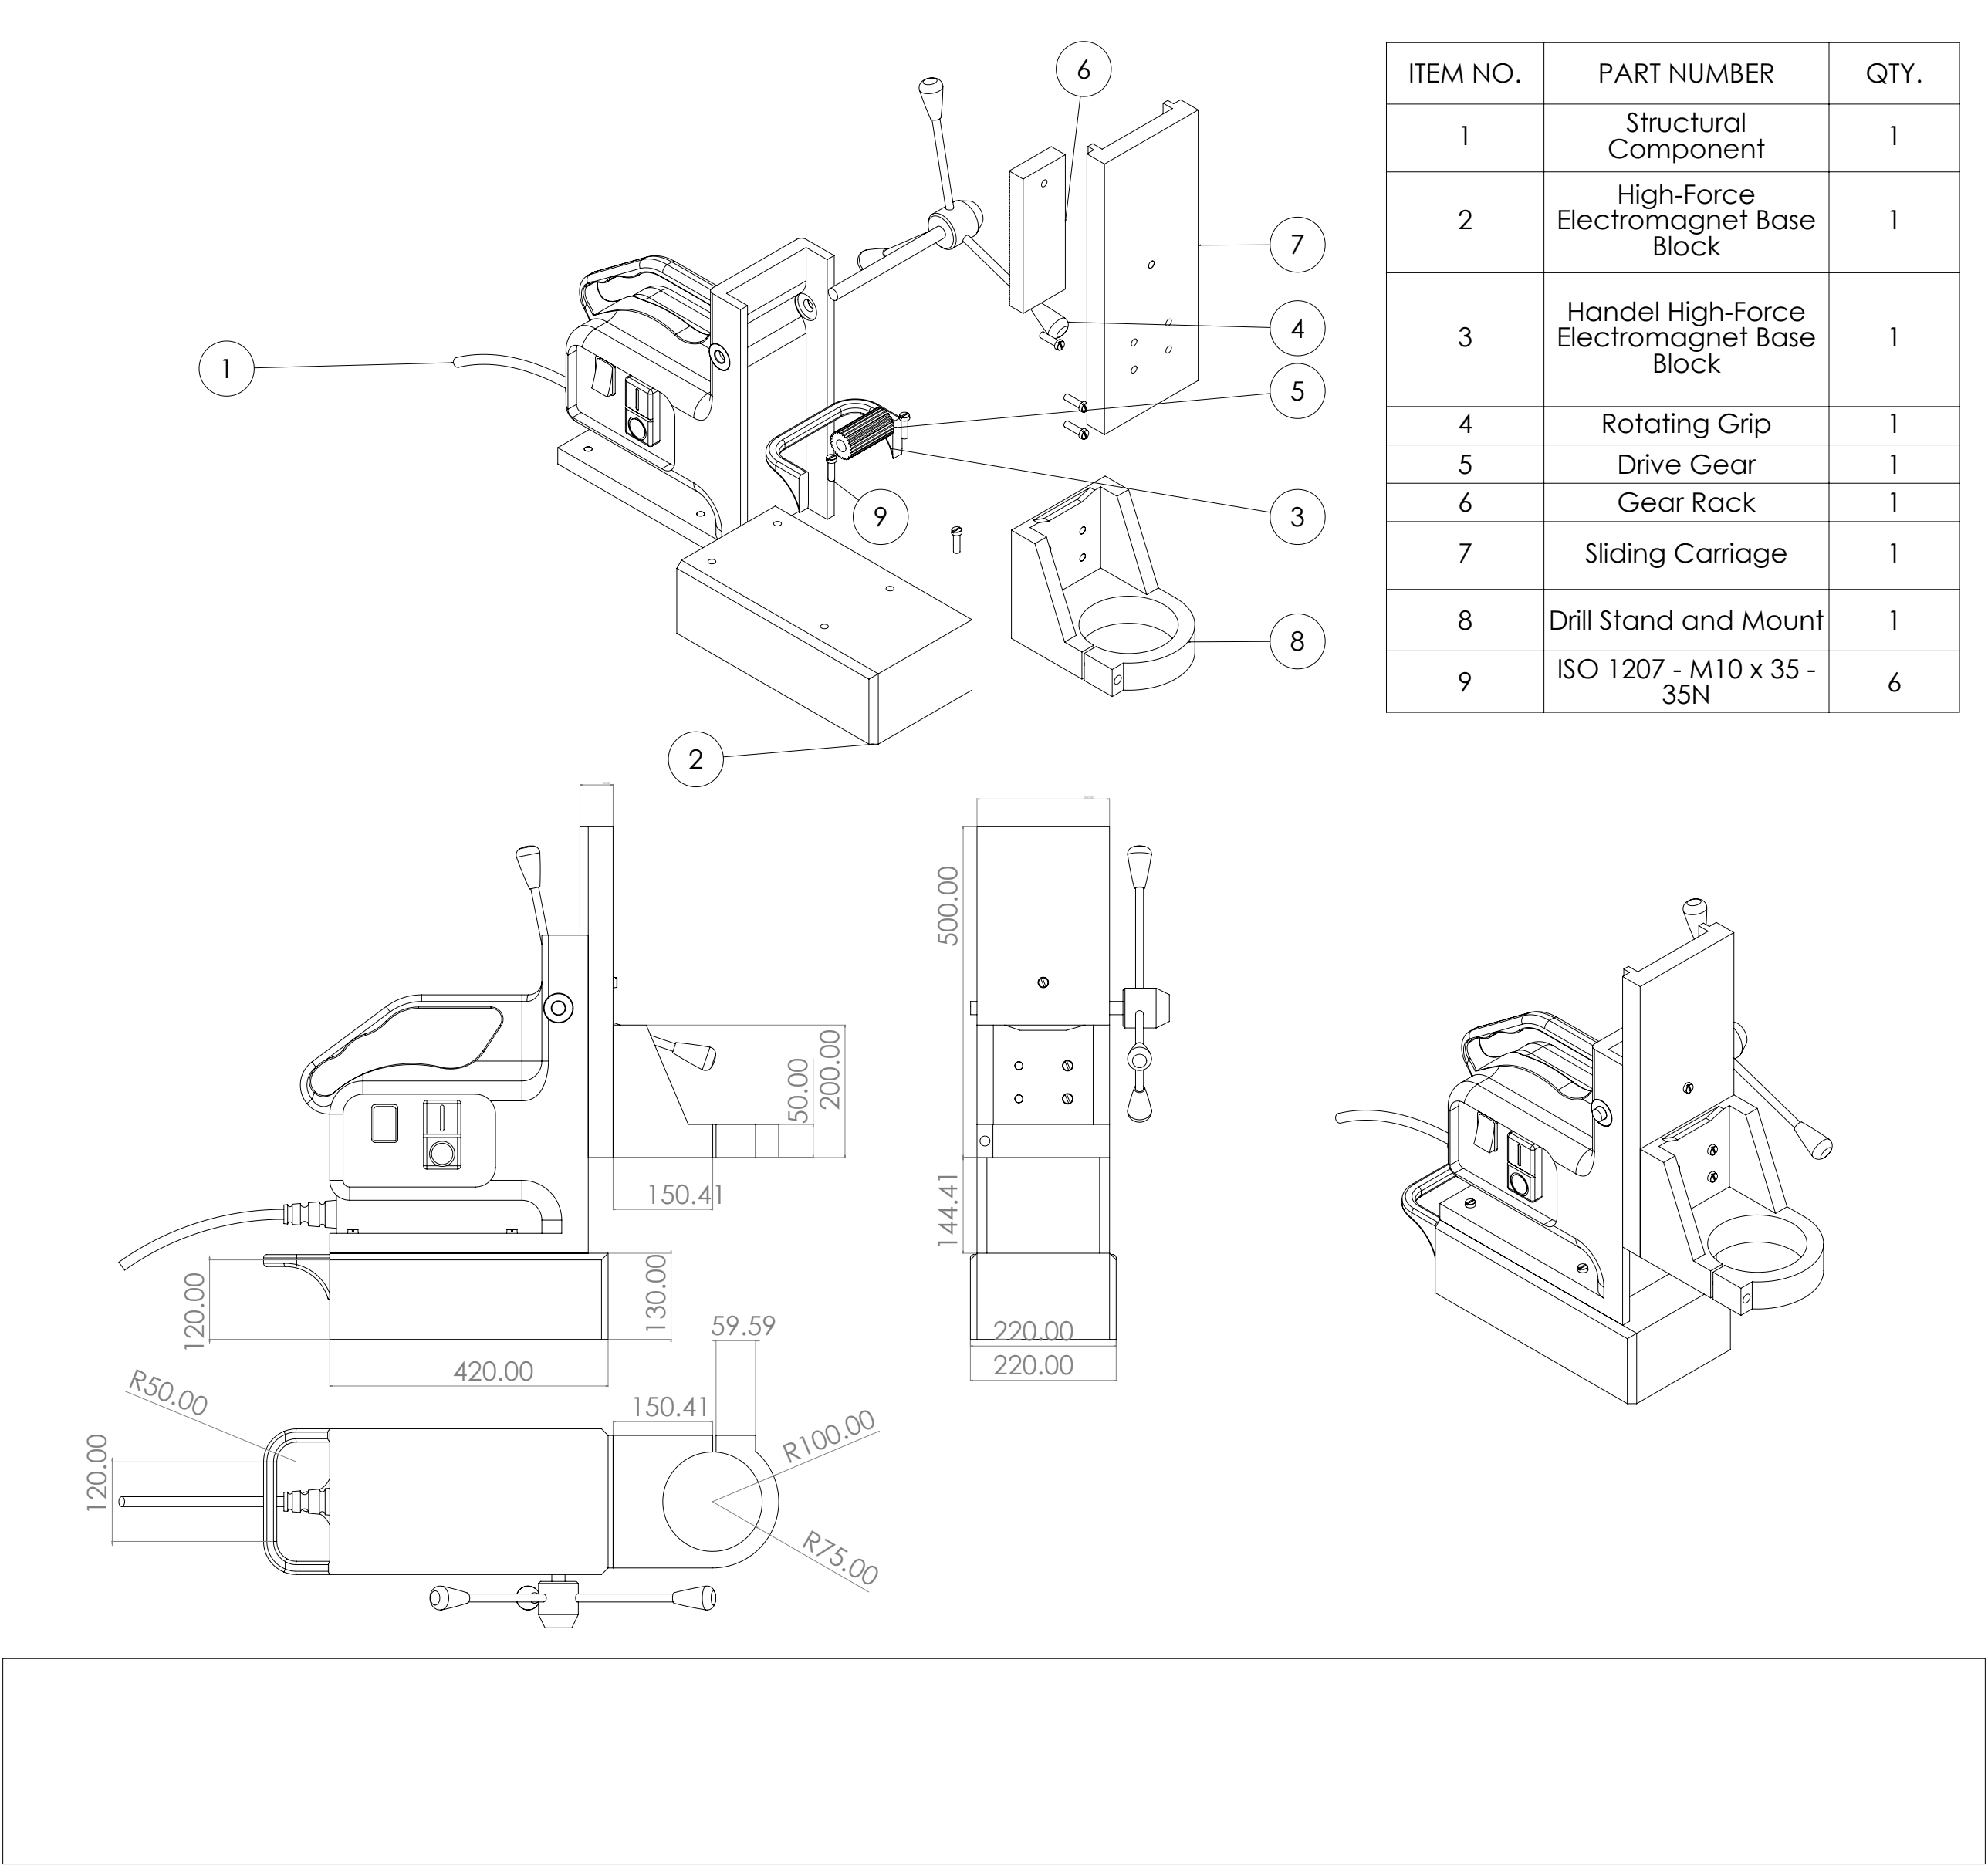
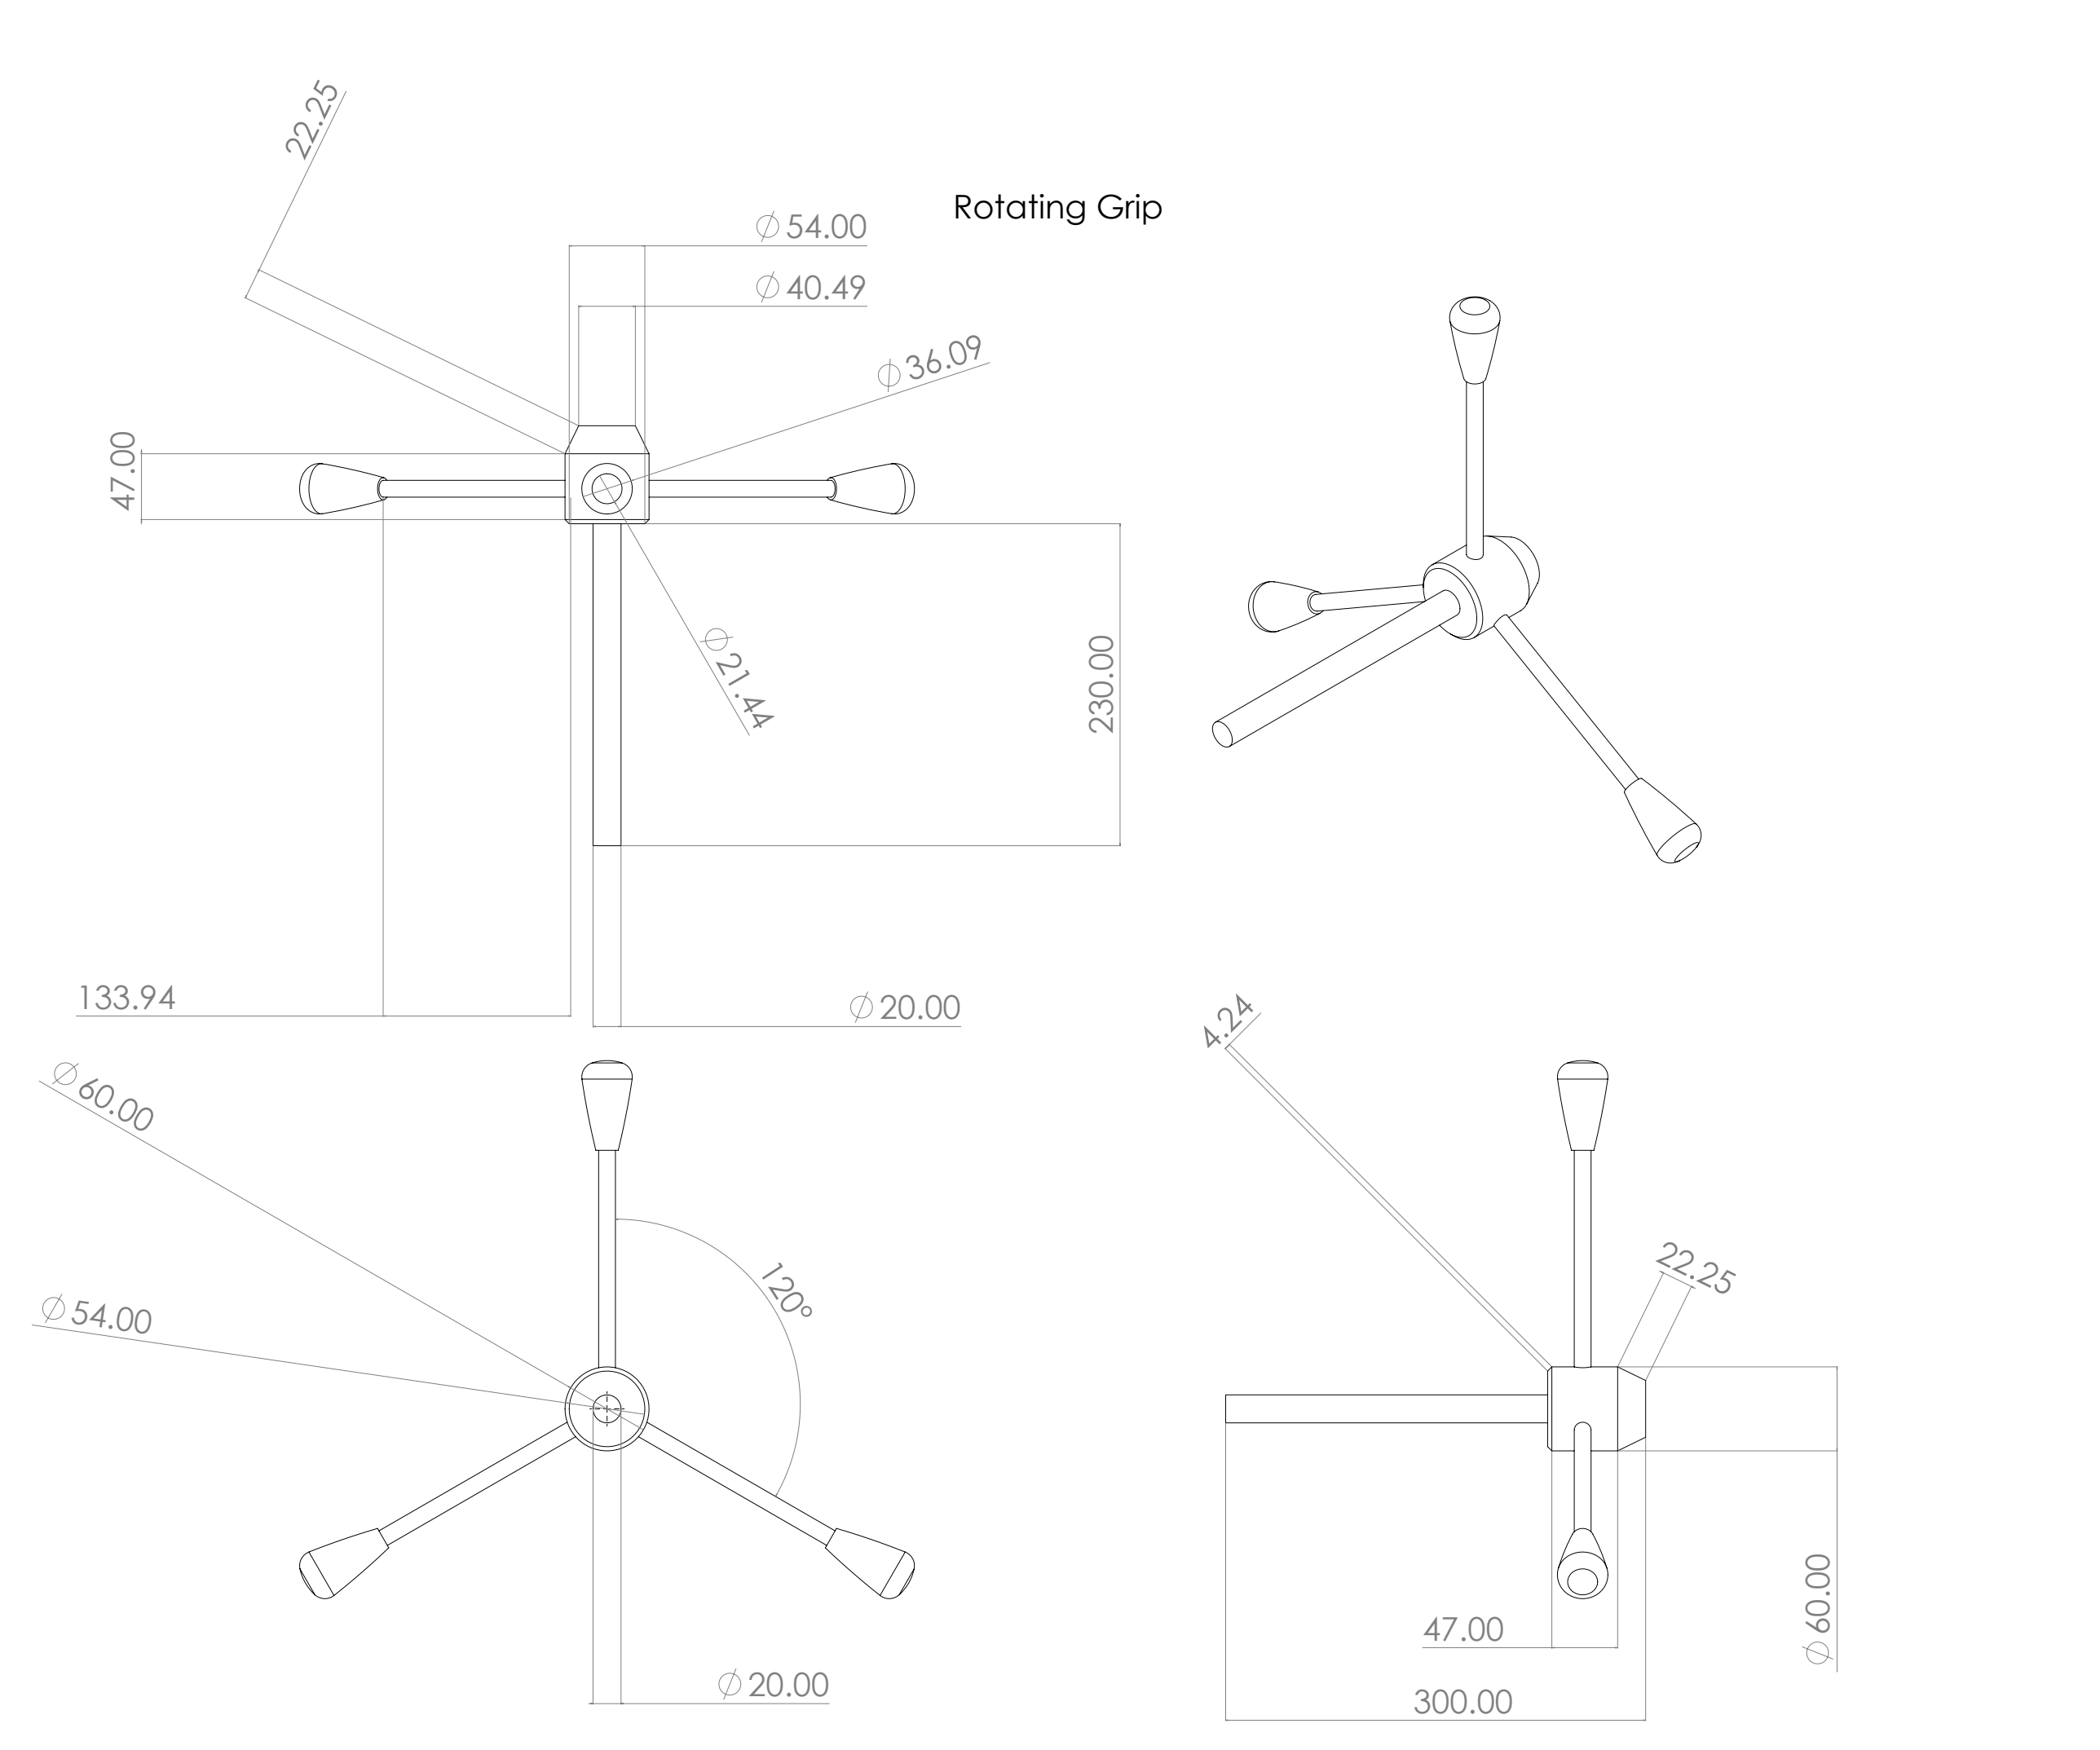
ISO-10303-21;
HEADER;
FILE_DESCRIPTION (('STEP AP214'),
    '1' );
FILE_NAME ('MAS-315',
    '2026-10-24T00:09:50',
    ( '' ),
    ( '' ),
    'SwSTEP 2.0',
    'SolidWorks 2025',
    '' );
FILE_SCHEMA (( 'AUTOMOTIVE_DESIGN' ));
ENDSEC;

DATA;
#1 = CARTESIAN_POINT ( 'NONE',  ( -209.5848783976569507, 66.48002492874486791, 33.34538701106990288 ) ) ;
#2 = CARTESIAN_POINT ( 'NONE',  ( 367.9108539694884144, 44.41075299063183479, 74.99887465166234790 ) ) ;
#3 = DIRECTION ( 'NONE',  ( 0.000000000000000000, 0.000000000000000000, 1.000000000000000000 ) ) ;
#5 = EDGE_LOOP ( 'NONE', ( #5978, #27245, #13781, #25937 ) ) ;
#4 = ORIENTED_EDGE ( 'NONE', *, *, #26664, .T. ) ;
#6 = CARTESIAN_POINT ( 'NONE',  ( -167.9302994091366088, 116.8073761394556271, 25.31690238253929337 ) ) ;
#7 = CARTESIAN_POINT ( 'NONE',  ( -110.7275636018716654, 68.51688903468615877, 83.00000000000001421 ) ) ;
#8 = ORIENTED_EDGE ( 'NONE', *, *, #11531, .F. ) ;
#9 = ADVANCED_FACE ( 'NONE', ( #20080 ), #15026, .T. ) ;
#10 = VERTEX_POINT ( 'NONE', #2127 ) ;
#11 = ORIENTED_EDGE ( 'NONE', *, *, #16841, .T. ) ;
#12 = EDGE_CURVE ( 'NONE', #4946, #18655, #10877, .T. ) ;
#13 = FACE_OUTER_BOUND ( 'NONE', #24456, .T. ) ;
#14 = VECTOR ( 'NONE', #24941, 1000.000000000000000 ) ;
#15 = DIRECTION ( 'NONE',  ( -1.850371707708594316E-16, 1.000000000000000000, 0.000000000000000000 ) ) ;
#16 = ORIENTED_EDGE ( 'NONE', *, *, #12011, .T. ) ;
#17 = DIRECTION ( 'NONE',  ( 6.123233995736816572E-17, 1.060575238724904203E-16, -1.000000000000000000 ) ) ;
#18 = AXIS2_PLACEMENT_3D ( 'NONE', #21734, #15134, #6353 ) ;
#19 = EDGE_CURVE ( 'NONE', #26943, #26049, #15367, .T. ) ;
#20 = CARTESIAN_POINT ( 'NONE',  ( 157.4999999999998579, 83.32081209086616980, 45.00000000000000000 ) ) ;
#21 = ORIENTED_EDGE ( 'NONE', *, *, #17846, .F. ) ;
#22 = CARTESIAN_POINT ( 'NONE',  ( -225.2031547890646266, 89.29438079543466245, 14.16277051160506417 ) ) ;
#23 = DIRECTION ( 'NONE',  ( 0.000000000000000000, 0.000000000000000000, -1.000000000000000000 ) ) ;
#24 = EDGE_CURVE ( 'NONE', #6807, #15188, #4704, .T. ) ;
#25 = CARTESIAN_POINT ( 'NONE',  ( 187.4999999999996305, 288.9665627064425166, 45.00000000000000000 ) ) ;
#26 = CARTESIAN_POINT ( 'NONE',  ( 160.9807621135329612, 204.9999999999998863, -151.0000000000000284 ) ) ;
#27 = ORIENTED_EDGE ( 'NONE', *, *, #22527, .F. ) ;
#28 = AXIS2_PLACEMENT_3D ( 'NONE', #2667, #6838, #19914 ) ;
#29 = CARTESIAN_POINT ( 'NONE',  ( 157.4999999999998579, 105.8916871584295478, 45.00000000000000000 ) ) ;
#30 = CARTESIAN_POINT ( 'NONE',  ( 158.0000000000016485, 50.46449948952111697, 45.00000000000000000 ) ) ;
#31 = LINE ( 'NONE', #28308, #26698 ) ;
#32 = DIRECTION ( 'NONE',  ( 0.000000000000000000, 1.387778780781445182E-16, -1.000000000000000000 ) ) ;
#33 = ORIENTED_EDGE ( 'NONE', *, *, #12258, .T. ) ;
#34 = EDGE_CURVE ( 'NONE', #22143, #25491, #9030, .T. ) ;
#35 = DIRECTION ( 'NONE',  ( -0.8916010070293783896, -0.4528218681382319422, 0.000000000000000000 ) ) ;
#36 = VECTOR ( 'NONE', #4972, 999.9999999999998863 ) ;
#37 = CARTESIAN_POINT ( 'NONE',  ( 158.0000000000006821, 140.7479997597746433, 45.00000000000000000 ) ) ;
#38 = DIRECTION ( 'NONE',  ( -1.541976423090495387E-16, 1.000000000000000000, -0.000000000000000000 ) ) ;
#39 = ORIENTED_EDGE ( 'NONE', *, *, #23270, .T. ) ;
#40 = EDGE_LOOP ( 'NONE', ( #25387, #6950, #12411, #9967 ) ) ;
#41 = EDGE_CURVE ( 'NONE', #5835, #23775, #13490, .T. ) ;
#42 = LINE ( 'NONE', #17847, #25312 ) ;
#43 = CARTESIAN_POINT ( 'NONE',  ( -192.2110555254130020, 101.5793329107164027, -32.81765284612617251 ) ) ;
#44 = EDGE_LOOP ( 'NONE', ( #26670, #4164, #18942, #22598 ) ) ;
#45 = ORIENTED_EDGE ( 'NONE', *, *, #2403, .F. ) ;
#46 = PLANE ( 'NONE',  #15936 ) ;
#47 = AXIS2_PLACEMENT_3D ( 'NONE', #22544, #2851, #8648 ) ;
#48 = FACE_OUTER_BOUND ( 'NONE', #22018, .T. ) ;
#49 = ORIENTED_EDGE ( 'NONE', *, *, #10620, .T. ) ;
#50 = EDGE_LOOP ( 'NONE', ( #21785, #9635, #7693, #13143 ) ) ;
#51 = LINE ( 'NONE', #15297, #1051 ) ;
#52 = EDGE_CURVE ( 'NONE', #5857, #12779, #18225, .T. ) ;
#53 = AXIS2_PLACEMENT_3D ( 'NONE', #26136, #19391, #25708 ) ;
#54 = EDGE_CURVE ( 'NONE', #1139, #21808, #13638, .T. ) ;
#55 = DIRECTION ( 'NONE',  ( 1.000000000000000000, 0.000000000000000000, 0.000000000000000000 ) ) ;
#56 = CARTESIAN_POINT ( 'NONE',  ( 158.0000000000000568, 203.4448749474510407, 45.00000000000000000 ) ) ;
#57 = CARTESIAN_POINT ( 'NONE',  ( 158.0000000000006821, 138.7479997597746433, 45.00000000000000000 ) ) ;
#58 = DIRECTION ( 'NONE',  ( -0.000000000000000000, -0.000000000000000000, -1.000000000000000000 ) ) ;
#59 = DIRECTION ( 'NONE',  ( -0.000000000000000000, -0.000000000000000000, -1.000000000000000000 ) ) ;
#60 = LINE ( 'NONE', #17580, #15416 ) ;
#61 = VERTEX_POINT ( 'NONE', #7448 ) ;
#62 = DIRECTION ( 'NONE',  ( 0.000000000000000000, 0.000000000000000000, 1.000000000000000000 ) ) ;
#63 = CARTESIAN_POINT ( 'NONE',  ( -112.3221550338875687, 74.54464929955099706, 83.00000000000001421 ) ) ;
#64 = FACE_OUTER_BOUND ( 'NONE', #25797, .T. ) ;
#65 = CARTESIAN_POINT ( 'NONE',  ( 157.4999999999998579, 93.35231212089433939, 45.00000000000000000 ) ) ;
#66 = ORIENTED_EDGE ( 'NONE', *, *, #15793, .T. ) ;
#67 = EDGE_CURVE ( 'NONE', #4321, #27397, #9743, .T. ) ;
#68 = CARTESIAN_POINT ( 'NONE',  ( 157.4999999999998579, 98.36806213590843129, -45.00000000000000000 ) ) ;
#69 = ORIENTED_EDGE ( 'NONE', *, *, #8545, .T. ) ;
#70 = VECTOR ( 'NONE', #14918, 1000.000000000000114 ) ;
#71 = DIRECTION ( 'NONE',  ( 1.321694076934710155E-16, -1.000000000000000000, 0.000000000000000000 ) ) ;
#72 = CARTESIAN_POINT ( 'NONE',  ( -242.2383635333241614, 73.34843395317835757, -5.047097023363151358 ) ) ;
#73 = CARTESIAN_POINT ( 'NONE',  ( -40.40953891503691153, 36.92584315232891612, 99.00000000000000000 ) ) ;
#74 = DIRECTION ( 'NONE',  ( 1.000000000000000000, -0.000000000000000000, -0.000000000000000000 ) ) ;
#75 = SURFACE_SIDE_STYLE ('',( #24494 ) ) ;
#76 = EDGE_LOOP ( 'NONE', ( #23237, #5440, #9626, #3047 ) ) ;
#77 = VECTOR ( 'NONE', #23464, 999.9999999999998863 ) ;
#78 = EDGE_CURVE ( 'NONE', #15009, #7688, #2981, .T. ) ;
#79 = VECTOR ( 'NONE', #3101, 1000.000000000000000 ) ;
#80 = DIRECTION ( 'NONE',  ( 0.000000000000000000, 0.000000000000000000, -1.000000000000000000 ) ) ;
#81 = ORIENTED_EDGE ( 'NONE', *, *, #14673, .T. ) ;
#82 = SPHERICAL_SURFACE ( 'NONE', #4853, 35.18636678425505693 ) ;
#83 = VERTEX_POINT ( 'NONE', #22814 ) ;
#84 = EDGE_CURVE ( 'NONE', #1460, #15527, #3074, .T. ) ;
#85 = ORIENTED_EDGE ( 'NONE', *, *, #17813, .T. ) ;
#86 = DIRECTION ( 'NONE',  ( 0.000000000000000000, 1.000000000000000000, -1.224646799147353207E-16 ) ) ;
#87 = ORIENTED_EDGE ( 'NONE', *, *, #18331, .F. ) ;
#88 = VERTEX_POINT ( 'NONE', #22953 ) ;
#89 = CARTESIAN_POINT ( 'NONE',  ( -260.0000000000001137, -157.0000000000000284, -109.9999999999998721 ) ) ;
#90 = CARTESIAN_POINT ( 'NONE',  ( 100.8286702512290418, 242.7181571222456284, 23.14229345413787442 ) ) ;
#91 = AXIS2_PLACEMENT_3D ( 'NONE', #3202, #20878, #24911 ) ;
#92 = DIRECTION ( 'NONE',  ( 0.8916010070295410372, -0.4528218681379115873, 0.000000000000000000 ) ) ;
#93 = CYLINDRICAL_SURFACE ( 'NONE', #27056, 5.999999999999991118 ) ;
#94 = AXIS2_PLACEMENT_3D ( 'NONE', #17993, #1165, #3172 ) ;
#95=STYLED_ITEM('',(#28448),#8854);
#96 = LINE ( 'NONE', #11159, #22961 ) ;
#97 = LINE ( 'NONE', #21929, #236 ) ;
#98 = CARTESIAN_POINT ( 'NONE',  ( -210.7172313291012529, 103.7585653882801182, 5.000000000000002665 ) ) ;
#99 = DIRECTION ( 'NONE',  ( -1.000000000000000000, 0.000000000000000000, 0.000000000000000000 ) ) ;
#100 = DIRECTION ( 'NONE',  ( 0.000000000000000000, -1.000000000000000000, 0.000000000000000000 ) ) ;
#101 = CARTESIAN_POINT ( 'NONE',  ( 134.9999999999998579, 220.0000000000000284, -99.00000000000001421 ) ) ;
#102 = LINE ( 'NONE', #19501, #15080 ) ;
#103 = DIRECTION ( 'NONE',  ( 0.5975062131282554700, -0.8018642810807398158, 0.000000000000000000 ) ) ;
#104 = ORIENTED_EDGE ( 'NONE', *, *, #18254, .F. ) ;
#105 = PLANE ( 'NONE',  #22522 ) ;
#106 = DIRECTION ( 'NONE',  ( 0.8916010070293283185, 0.4528218681383305855, 0.000000000000000000 ) ) ;
#107 = CARTESIAN_POINT ( 'NONE',  ( 158.0000000000012221, 88.59049960963380954, -45.00000000000000000 ) ) ;
#108 = CARTESIAN_POINT ( 'NONE',  ( 107.6462301271458841, 207.6792144784505467, -139.8040206391607398 ) ) ;
#109 = EDGE_CURVE ( 'NONE', #28186, #27342, #11484, .T. ) ;
#110 = ORIENTED_EDGE ( 'NONE', *, *, #7705, .T. ) ;
#111 = EDGE_CURVE ( 'NONE', #4742, #22382, #9467, .T. ) ;
#112 = VECTOR ( 'NONE', #9793, 1000.000000000000000 ) ;
#113 = CARTESIAN_POINT ( 'NONE',  ( 338.9795809418241106, 102.2323340340494724, -145.0000000000000000 ) ) ;
#114 = EDGE_LOOP ( 'NONE', ( #13763, #3696, #24044, #20717 ) ) ;
#115 = CARTESIAN_POINT ( 'NONE',  ( -25.41017935548559947, 129.2224694249450181, -15.66087358766781534 ) ) ;
#116 = ORIENTED_EDGE ( 'NONE', *, *, #27781, .F. ) ;
#117 = VECTOR ( 'NONE', #24571, 1000.000000000000114 ) ;
#118 = ORIENTED_EDGE ( 'NONE', *, *, #15885, .F. ) ;
#119 = CIRCLE ( 'NONE', #12970, 75.00000000000002842 ) ;
#120 = ORIENTED_EDGE ( 'NONE', *, *, #25163, .F. ) ;
#121 = ORIENTED_EDGE ( 'NONE', *, *, #12188, .T. ) ;
#122 = DIRECTION ( 'NONE',  ( -1.850371707708594316E-16, 1.000000000000000000, -0.000000000000000000 ) ) ;
#123 = DIRECTION ( 'NONE',  ( 0.8916010070293710621, -0.4528218681382463195, 0.000000000000000000 ) ) ;
#124 = EDGE_CURVE ( 'NONE', #26591, #26642, #21635, .T. ) ;
#125 = PLANE ( 'NONE',  #22915 ) ;
#126 = DIRECTION ( 'NONE',  ( -1.000000000000000000, 0.000000000000000000, 0.000000000000000000 ) ) ;
#127 = VECTOR ( 'NONE', #25950, 1000.000000000000000 ) ;
#128 = CARTESIAN_POINT ( 'NONE',  ( -216.1549772618016334, 59.20708407665082262, 28.62293862808999734 ) ) ;
#129 = LINE ( 'NONE', #12656, #21109 ) ;
#130 = CARTESIAN_POINT ( 'NONE',  ( 217.4999999999996305, -5.589247009368136787, -100.0000000000000142 ) ) ;
#131 = VECTOR ( 'NONE', #4235, 1000.000000000000000 ) ;
#132 = ADVANCED_FACE ( 'NONE', ( #14200 ), #4989, .F. ) ;
#133 = DIRECTION ( 'NONE',  ( 0.000000000000000000, 0.000000000000000000, 1.000000000000000000 ) ) ;
#134 = DIRECTION ( 'NONE',  ( -8.673617379884073683E-17, -1.000000000000000000, 0.000000000000000000 ) ) ;
#135 = CIRCLE ( 'NONE', #13922, 19.07743405327024888 ) ;
#136 = CARTESIAN_POINT ( 'NONE',  ( -203.1779787704217313, 93.05164332230201296, -28.77272332722132475 ) ) ;
#137 = FACE_OUTER_BOUND ( 'NONE', #15642, .T. ) ;
#138 = VECTOR ( 'NONE', #24642, 1000.000000000000000 ) ;
#139 = DIRECTION ( 'NONE',  ( 0.000000000000000000, 0.000000000000000000, 1.000000000000000000 ) ) ;
#140 = FACE_OUTER_BOUND ( 'NONE', #22475, .T. ) ;
#141 = CARTESIAN_POINT ( 'NONE',  ( 65.00000000000000000, -170.0000000000000853, -64.00000000000001421 ) ) ;
#142 = EDGE_CURVE ( 'NONE', #11100, #5099, #795, .T. ) ;
#143 = LINE ( 'NONE', #23706, #15280 ) ;
#144 = AXIS2_PLACEMENT_3D ( 'NONE', #11987, #2630, #13865 ) ;
#146 = ORIENTED_EDGE ( 'NONE', *, *, #9436, .T. ) ;
#145 = ORIENTED_EDGE ( 'NONE', *, *, #16814, .F. ) ;
#147 = LINE ( 'NONE', #4014, #25212 ) ;
#148 = EDGE_CURVE ( 'NONE', #2800, #8056, #19588, .T. ) ;
#149 = EDGE_CURVE ( 'NONE', #7691, #16820, #7209, .T. ) ;
#150 = DIRECTION ( 'NONE',  ( 0.000000000000000000, -1.000000000000000000, 0.000000000000000000 ) ) ;
#151 = ORIENTED_EDGE ( 'NONE', *, *, #11275, .F. ) ;
#152 = VERTEX_POINT ( 'NONE', #25244 ) ;
#153 = VECTOR ( 'NONE', #12581, 1000.000000000000000 ) ;
#154 = ORIENTED_EDGE ( 'NONE', *, *, #16207, .F. ) ;
#155 = TOROIDAL_SURFACE ( 'NONE', #2900, 39.99999999999999289, 9.999999999999996447 ) ;
#156 = DIRECTION ( 'NONE',  ( 0.000000000000000000, 0.000000000000000000, -1.000000000000000000 ) ) ;
#157 = CARTESIAN_POINT ( 'NONE',  ( -107.7774523778934253, 133.6573832689441019, 15.67481254453494088 ) ) ;
#158 = ORIENTED_EDGE ( 'NONE', *, *, #7014, .F. ) ;
#159 = AXIS2_PLACEMENT_3D ( 'NONE', #7876, #3416, #12207 ) ;
#160 = CARTESIAN_POINT ( 'NONE',  ( 94.38583646779612479, 113.6320904522268336, -99.99999999997839950 ) ) ;
#161 = CARTESIAN_POINT ( 'NONE',  ( 157.9999999999996589, 279.1890001801680796, 45.00000000000000000 ) ) ;
#162 = ORIENTED_EDGE ( 'NONE', *, *, #25176, .F. ) ;
#163 = CARTESIAN_POINT ( 'NONE',  ( -209.0375512581602493, 88.61097887464748624, 26.00739845333608358 ) ) ;
#164 = CARTESIAN_POINT ( 'NONE',  ( -211.9382648910248861, -218.8137564101509724, 107.3933716542343575 ) ) ;
#165 = CARTESIAN_POINT ( 'NONE',  ( -205.7061355896894383, 146.0477147645469813, 12.99999999999999822 ) ) ;
#166 = CARTESIAN_POINT ( 'NONE',  ( 158.4246112489018401, 201.2552156260056222, -141.0358260266776540 ) ) ;
#167 = VECTOR ( 'NONE', #6302, 1000.000000000000000 ) ;
#168 = ADVANCED_FACE ( 'NONE', ( #27523 ), #5563, .T. ) ;
#169 = EDGE_CURVE ( 'NONE', #1220, #7618, #16907, .T. ) ;
#170 = VERTEX_POINT ( 'NONE', #23513 ) ;
#171 = AXIS2_PLACEMENT_3D ( 'NONE', #10028, #18512, #2846 ) ;
#172 = DIRECTION ( 'NONE',  ( 0.8916010070298353574, -0.4528218681373320509, 0.000000000000000000 ) ) ;
#173 = ADVANCED_FACE ( 'NONE', ( #5707 ), #18920, .T. ) ;
#174 = CARTESIAN_POINT ( 'NONE',  ( 158.0000000000004832, 161.3188748273380213, 45.00000000000000000 ) ) ;
#175 = CYLINDRICAL_SURFACE ( 'NONE', #3295, 5.000000000000004441 ) ;
#176 = VECTOR ( 'NONE', #1198, 1000.000000000000000 ) ;
#177 = CARTESIAN_POINT ( 'NONE',  ( 48.45469728424487244, 192.9461374953035033, 12.99999999999999822 ) ) ;
#178 = EDGE_LOOP ( 'NONE', ( #23936, #17457 ) ) ;
#179 = LINE ( 'NONE', #13127, #5008 ) ;
#180 = ADVANCED_FACE ( 'NONE', ( #3827 ), #7726, .F. ) ;
#181 = CARTESIAN_POINT ( 'NONE',  ( 217.4999999999996305, 133.0668745871126930, -36.86484227207694886 ) ) ;
#182 = LINE ( 'NONE', #19713, #24117 ) ;
#183 = ORIENTED_EDGE ( 'NONE', *, *, #24834, .F. ) ;
#184 = DIRECTION ( 'NONE',  ( 0.000000000000000000, 0.000000000000000000, 1.000000000000000000 ) ) ;
#185 = ORIENTED_EDGE ( 'NONE', *, *, #10567, .T. ) ;
#186 = PRODUCT_DEFINITION ( 'UNKNOWN', '', #23049, #8609 ) ;
#187 = DIRECTION ( 'NONE',  ( 0.000000000000000000, 0.000000000000000000, 1.000000000000000000 ) ) ;
#188 = CARTESIAN_POINT ( 'NONE',  ( -196.6905515939650400, 98.40619709718011165, -31.75569965019813523 ) ) ;
#189 = EDGE_LOOP ( 'NONE', ( #11478, #20043, #1558, #19553 ) ) ;
#190 = VECTOR ( 'NONE', #9323, 1000.000000000000227 ) ;
#191 = ORIENTED_EDGE ( 'NONE', *, *, #11968, .F. ) ;
#192 = CARTESIAN_POINT ( 'NONE',  ( -111.8131014667890213, 70.11474204378114905, 82.89209462293977992 ) ) ;
#193 = CARTESIAN_POINT ( 'NONE',  ( 109.9999999999998863, 330.0000000000000000, 90.00000000000002842 ) ) ;
#194 = VERTEX_POINT ( 'NONE', #10023 ) ;
#195 = ORIENTED_EDGE ( 'NONE', *, *, #27994, .T. ) ;
#196 = VECTOR ( 'NONE', #16989, 1000.000000000000000 ) ;
#197 = CARTESIAN_POINT ( 'NONE',  ( -200.0000000000000284, -91.18033988749901653, 21.20097097723064294 ) ) ;
#198 = DIRECTION ( 'NONE',  ( 0.000000000000000000, 0.000000000000000000, -1.000000000000000000 ) ) ;
#199 = CARTESIAN_POINT ( 'NONE',  ( 157.4999999999997442, 253.8563126013445697, -45.00000000000000000 ) ) ;
#200 = CARTESIAN_POINT ( 'NONE',  ( 158.0000000000017053, 45.44874947450702507, 45.00000000000000000 ) ) ;
#201 = SHAPE_REPRESENTATION ( 'Rotating Grip', ( #10637 ), #10190 ) ;
#202 = LINE ( 'NONE', #25668, #4520 ) ;
#203 = CARTESIAN_POINT ( 'NONE',  ( -209.9813599551185916, 61.38898174817780529, -24.60129468178291035 ) ) ;
#204 = CARTESIAN_POINT ( 'NONE',  ( -63.57415822541634043, -18.01420295945611727, 95.00000000000000000 ) ) ;
#205 = EDGE_CURVE ( 'NONE', #9863, #2501, #3463, .T. ) ;
#206 = EDGE_CURVE ( 'NONE', #17779, #12189, #27834, .T. ) ;
#207 = EDGE_LOOP ( 'NONE', ( #12910, #1760, #26526, #6163 ) ) ;
#208 = LINE ( 'NONE', #21895, #12696 ) ;
#209 = DIRECTION ( 'NONE',  ( 0.000000000000000000, 0.000000000000000000, -1.000000000000000000 ) ) ;
#210 = CARTESIAN_POINT ( 'NONE',  ( 184.9999999999999432, 330.0000000000000000, 84.99999999999995737 ) ) ;
#211 = CARTESIAN_POINT ( 'NONE',  ( -260.0000000000001137, -220.0000000000000853, 110.0000000000000142 ) ) ;
#212 = VERTEX_POINT ( 'NONE', #12332 ) ;
#213 = AXIS2_PLACEMENT_3D ( 'NONE', #16151, #24903, #909 ) ;
#214 = CARTESIAN_POINT ( 'NONE',  ( 232.4999999999996305, 133.0668745871126930, 36.86484227207694886 ) ) ;
#215 = EDGE_LOOP ( 'NONE', ( #22439, #1141, #3307, #4955, #12631, #20188 ) ) ;
#216 = CARTESIAN_POINT ( 'NONE',  ( 158.0000000000001421, 191.4133749174225443, 45.00000000000000000 ) ) ;
#217 = LINE ( 'NONE', #22769, #1813 ) ;
#218 = DIRECTION ( 'NONE',  ( -1.541976423090495387E-16, 1.000000000000000000, 0.000000000000000000 ) ) ;
#219 = ORIENTED_EDGE ( 'NONE', *, *, #15468, .T. ) ;
#220 = FILL_AREA_STYLE ('',( #11139 ) ) ;
#221 = SURFACE_STYLE_USAGE ( .BOTH. , #75 ) ;
#222 = VECTOR ( 'NONE', #16891, 1000.000000000000000 ) ;
#223 = VERTEX_POINT ( 'NONE', #1394 ) ;
#224 = ADVANCED_FACE ( 'NONE', ( #25661 ), #17044, .F. ) ;
#225 = CARTESIAN_POINT ( 'NONE',  ( -210.1746890037166793, 73.83603441591317562, 34.06685219078467242 ) ) ;
#226 = VERTEX_POINT ( 'NONE', #23659 ) ;
#227 = ADVANCED_FACE ( 'NONE', ( #3967, #12753 ), #21493, .F. ) ;
#228 = FACE_OUTER_BOUND ( 'NONE', #26705, .T. ) ;
#229 = ORIENTED_EDGE ( 'NONE', *, *, #19889, .T. ) ;
#230 = VERTEX_POINT ( 'NONE', #6412 ) ;
#231 = DIRECTION ( 'NONE',  ( 1.000000000000000000, 0.000000000000000000, -0.000000000000000000 ) ) ;
#232 = VECTOR ( 'NONE', #17902, 1000.000000000000000 ) ;
#233 = ORIENTED_EDGE ( 'NONE', *, *, #12489, .T. ) ;
#234 = EDGE_LOOP ( 'NONE', ( #15831, #2366, #304, #19218 ) ) ;
#235 = CARTESIAN_POINT ( 'NONE',  ( -220.9647007329185158, 136.4514858755404987, 12.97939780113086705 ) ) ;
#236 = VECTOR ( 'NONE', #2100, 1000.000000000000000 ) ;
#237 = VECTOR ( 'NONE', #8756, 1000.000000000000000 ) ;
#238 = ADVANCED_FACE ( 'NONE', ( #10870 ), #21904, .F. ) ;
#239 = CARTESIAN_POINT ( 'NONE',  ( 103.5789823554282947, 245.2557385300782471, 18.86932834259753733 ) ) ;
#240 = EDGE_CURVE ( 'NONE', #11439, #27657, #27406, .T. ) ;
#241 = DIRECTION ( 'NONE',  ( -0.8660254037844362651, 0.5000000000000039968, -0.000000000000000000 ) ) ;
#242 = DIRECTION ( 'NONE',  ( 0.000000000000000000, 0.000000000000000000, 1.000000000000000000 ) ) ;
#243 = AXIS2_PLACEMENT_3D ( 'NONE', #5659, #16167, #3495 ) ;
#244 = DIRECTION ( 'NONE',  ( -0.000000000000000000, -0.000000000000000000, -1.000000000000000000 ) ) ;
#245 = CARTESIAN_POINT ( 'NONE',  ( -260.0000000000001137, -165.0000000000001137, 60.00000000000002132 ) ) ;
#246 = DIRECTION ( 'NONE',  ( 0.8660254037844432595, 0.4999999999999919509, -0.000000000000000000 ) ) ;
#247 = CARTESIAN_POINT ( 'NONE',  ( 158.0000000000007674, 133.2243747372535267, -45.00000000000000000 ) ) ;
#248 = CARTESIAN_POINT ( 'NONE',  ( 158.0000000000003411, 173.8582498648732440, -45.00000000000000000 ) ) ;
#249 = LINE ( 'NONE', #6703, #21167 ) ;
#250 = DIRECTION ( 'NONE',  ( 8.659560562354934091E-17, 0.7071067811865474617, -0.7071067811865476838 ) ) ;
#251 = CARTESIAN_POINT ( 'NONE',  ( 432.4999999999996589, 44.41075299063184190, 75.99342076785332267 ) ) ;
#252 = ORIENTED_EDGE ( 'NONE', *, *, #25685, .T. ) ;
#253 = DIRECTION ( 'NONE',  ( 0.4163300014277677707, -0.9092135777204137792, 0.000000000000000000 ) ) ;
#254 = FACE_OUTER_BOUND ( 'NONE', #27282, .T. ) ;
#255 = DIRECTION ( 'NONE',  ( 0.000000000000000000, 0.000000000000000000, -1.000000000000000000 ) ) ;
#256 = CARTESIAN_POINT ( 'NONE',  ( 107.3811808525395151, 208.2821736267427752, -140.2307156351394610 ) ) ;
#257 = EDGE_LOOP ( 'NONE', ( #18040, #22551, #6751, #26799 ) ) ;
#258 = VECTOR ( 'NONE', #9581, 1000.000000000000000 ) ;
#259 = EDGE_CURVE ( 'NONE', #1752, #10216, #14126, .T. ) ;
#260 = CARTESIAN_POINT ( 'NONE',  ( 367.9108539694884144, 19.41075299063184900, 87.99671038392668265 ) ) ;
#261 = ORIENTED_EDGE ( 'NONE', *, *, #205, .F. ) ;
#262 = DIRECTION ( 'NONE',  ( -0.000000000000000000, -1.024644424698391667E-16, 1.000000000000000000 ) ) ;
#263 = ORIENTED_EDGE ( 'NONE', *, *, #21022, .F. ) ;
#264 = AXIS2_PLACEMENT_3D ( 'NONE', #19395, #6183, #2008 ) ;
#265 = ORIENTED_EDGE ( 'NONE', *, *, #8156, .T. ) ;
#266 = ORIENTED_EDGE ( 'NONE', *, *, #2989, .F. ) ;
#267 = ORIENTED_EDGE ( 'NONE', *, *, #6042, .T. ) ;
#268 = VERTEX_POINT ( 'NONE', #24222 ) ;
#269 = DIRECTION ( 'NONE',  ( 0.000000000000000000, 0.000000000000000000, 1.000000000000000000 ) ) ;
#270 = CARTESIAN_POINT ( 'NONE',  ( -180.0000000000000284, -40.00000000000004974, 70.00000000000001421 ) ) ;
#271 = CARTESIAN_POINT ( 'NONE',  ( 157.4999999999998579, 183.6358123911478799, 45.00000000000000000 ) ) ;
#272 = DIRECTION ( 'NONE',  ( 0.000000000000000000, 0.000000000000000000, -1.000000000000000000 ) ) ;
#273 = VECTOR ( 'NONE', #6730, 1000.000000000000000 ) ;
#274 = PRODUCT_DEFINITION_CONTEXT ( 'detailed design', #21209, 'design' ) ;
#276 = EDGE_CURVE ( 'NONE', #11934, #27327, #6832, .T. ) ;
#275 = VECTOR ( 'NONE', #1072, 1000.000000000000000 ) ;
#277 = FACE_OUTER_BOUND ( 'NONE', #22057, .T. ) ;
#278 = EDGE_CURVE ( 'NONE', #18107, #2726, #15475, .T. ) ;
#279 = CARTESIAN_POINT ( 'NONE',  ( -212.2468527728169931, 60.00277588997245459, 15.59298365948827225 ) ) ;
#280 = CARTESIAN_POINT ( 'NONE',  ( 176.1454027868280434, 57.48855481560072889, -45.00000000000000000 ) ) ;
#281 = PLANE ( 'NONE',  #14960 ) ;
#282 = B_SPLINE_CURVE_WITH_KNOTS ( 'NONE', 3,
 ( #2142, #28138, #4579, #11204, #26414, #10916, #13506, #17233, #1, #2281, #25992, #19677, #22257, #19813, #6311, #13087, #23849, #13365 ),
 .UNSPECIFIED., .F., .F.,
 ( 4, 2, 2, 2, 2, 2, 2, 2, 4 ),
 ( -3.464102035643382632E-05, 0.004053789758800030972, 0.008142220537956495682, 0.01223065131711295953, 0.01631908209626942510, 0.02449594365458239789, 0.02654015904416063762, 0.02858437443373887041, 0.03267280521289535333 ),
 .UNSPECIFIED. ) ;
#283 = LINE ( 'NONE', #20091, #23680 ) ;
#284 = CARTESIAN_POINT ( 'NONE',  ( 157.4999999999998579, 163.5728123310915407, 45.00000000000000000 ) ) ;
#285 = ADVANCED_FACE ( 'NONE', ( #4393 ), #15978, .T. ) ;
#286 = AXIS2_PLACEMENT_3D ( 'NONE', #20944, #11920, #18789 ) ;
#287 = LINE ( 'NONE', #25846, #26979 ) ;
#288 = DIRECTION ( 'NONE',  ( -1.321694076934710155E-16, 1.000000000000000000, 0.000000000000000000 ) ) ;
#289 = LINE ( 'NONE', #2568, #5884 ) ;
#290 = CARTESIAN_POINT ( 'NONE',  ( 111.3836151241014960, 219.3130464734738325, 45.00000000000000000 ) ) ;
#291 = CARTESIAN_POINT ( 'NONE',  ( -160.0000000000000284, 119.7660240611718763, 22.85081902853005431 ) ) ;
#292 = DIRECTION ( 'NONE',  ( 1.000000000000000000, 0.000000000000000000, 0.000000000000000000 ) ) ;
#294 = ORIENTED_EDGE ( 'NONE', *, *, #2530, .T. ) ;
#293 = ORIENTED_EDGE ( 'NONE', *, *, #15468, .F. ) ;
#295 = CARTESIAN_POINT ( 'NONE',  ( -222.7702326850704821, 86.58333552780506182, -17.42169760653345634 ) ) ;
#296 = DIRECTION ( 'NONE',  ( -0.000000000000000000, -0.000000000000000000, -1.000000000000000000 ) ) ;
#297 = CARTESIAN_POINT ( 'NONE',  ( -204.4166662746044665, 91.57150914865317759, -29.20755859028324508 ) ) ;
#298 = ORIENTED_EDGE ( 'NONE', *, *, #15430, .T. ) ;
#299 = ORIENTED_EDGE ( 'NONE', *, *, #27948, .T. ) ;
#300 = VECTOR ( 'NONE', #28359, 1000.000000000000000 ) ;
#301 = VERTEX_POINT ( 'NONE', #89 ) ;
#302 = LINE ( 'NONE', #15395, #9767 ) ;
#303 = CARTESIAN_POINT ( 'NONE',  ( -156.4144565615572731, 122.2051147660285579, 19.70699073531202572 ) ) ;
#304 = ORIENTED_EDGE ( 'NONE', *, *, #26732, .T. ) ;
#305 = AXIS2_PLACEMENT_3D ( 'NONE', #16749, #21045, #18753 ) ;
#306 = ORIENTED_EDGE ( 'NONE', *, *, #8739, .F. ) ;
#307 = CARTESIAN_POINT ( 'NONE',  ( 157.4999999999996589, 276.4271876689075498, 45.00000000000000000 ) ) ;
#308 = CYLINDRICAL_SURFACE ( 'NONE', #13262, 19.07743405327024888 ) ;
#309 = ORIENTED_EDGE ( 'NONE', *, *, #678, .T. ) ;
#310 = ADVANCED_FACE ( 'NONE', ( #4526 ), #6410, .T. ) ;
#311 = CARTESIAN_POINT ( 'NONE',  ( -207.4306580894464389, 90.17638659202999918, 25.66226923892150324 ) ) ;
#312 = CARTESIAN_POINT ( 'NONE',  ( -213.1827219047386848, -216.7767438708612531, 105.0000000000000142 ) ) ;
#313 = EDGE_CURVE ( 'NONE', #4881, #7087, #25948, .T. ) ;
#314 = ADVANCED_FACE ( 'NONE', ( #8712 ), #4110, .F. ) ;
#315 = ADVANCED_FACE ( 'NONE', ( #3468 ), #14543, .F. ) ;
#316 = CARTESIAN_POINT ( 'NONE',  ( 134.9999999999998579, 220.0000000000000284, -122.9999999999999574 ) ) ;
#317 = FACE_OUTER_BOUND ( 'NONE', #2935, .T. ) ;
#318 = CIRCLE ( 'NONE', #8106, 1.999999999999994893 ) ;
#319 = CARTESIAN_POINT ( 'NONE',  ( -218.1276041038538551, 59.80742093790404112, -25.66002785714302803 ) ) ;
#320 = ORIENTED_EDGE ( 'NONE', *, *, #18339, .T. ) ;
#321 = PLANE ( 'NONE',  #16025 ) ;
#322 = CARTESIAN_POINT ( 'NONE',  ( -225.9601317720483280, 132.4444111280268430, -15.07876772300364010 ) ) ;
#323 = DIRECTION ( 'NONE',  ( 0.000000000000000000, 0.000000000000000000, 1.000000000000000000 ) ) ;
#324 = CARTESIAN_POINT ( 'NONE',  ( 134.6436608991879496, 206.7391133850113079, 45.00000000000000000 ) ) ;
#325 = EDGE_LOOP ( 'NONE', ( #25386, #12742, #27550, #6157 ) ) ;
#326 = DIRECTION ( 'NONE',  ( -0.8916010070300282031, 0.4528218681369524101, 0.000000000000000000 ) ) ;
#327 = FACE_OUTER_BOUND ( 'NONE', #2294, .T. ) ;
#328 = CARTESIAN_POINT ( 'NONE',  ( -138.6428522700808230, 71.54464929955099706, 82.80879831960034210 ) ) ;
#329 = ORIENTED_EDGE ( 'NONE', *, *, #12094, .T. ) ;
#330 = ORIENTED_EDGE ( 'NONE', *, *, #4768, .T. ) ;
#331 = DIRECTION ( 'NONE',  ( -0.6343833064826072121, 0.7730186417261841747, 0.000000000000000000 ) ) ;
#332 = CARTESIAN_POINT ( 'NONE',  ( 0.000000000000000000, 0.000000000000000000, 100.0000000000000000 ) ) ;
#333 = ORIENTED_EDGE ( 'NONE', *, *, #4508, .T. ) ;
#334 = VECTOR ( 'NONE', #5178, 1000.000000000000000 ) ;
#335 = ORIENTED_EDGE ( 'NONE', *, *, #12580, .F. ) ;
#336 = FACE_OUTER_BOUND ( 'NONE', #23638, .T. ) ;
#337 = ADVANCED_FACE ( 'NONE', ( #27449 ), #5770, .T. ) ;
#338 = EDGE_CURVE ( 'NONE', #14636, #5476, #7520, .T. ) ;
#339 = DIRECTION ( 'NONE',  ( 0.000000000000000000, 0.000000000000000000, 1.000000000000000000 ) ) ;
#340 = EDGE_LOOP ( 'NONE', ( #7547, #3673, #5689, #22912 ) ) ;
#341 = ORIENTED_EDGE ( 'NONE', *, *, #16850, .F. ) ;
#342 = DIRECTION ( 'NONE',  ( 1.000000000000000000, 0.000000000000000000, 0.000000000000000000 ) ) ;
#343 = ADVANCED_FACE ( 'NONE', ( #765 ), #3046, .F. ) ;
#344 = ADVANCED_FACE ( 'NONE', ( #18569 ), #902, .F. ) ;
#345 = FACE_OUTER_BOUND ( 'NONE', #10535, .T. ) ;
#346 = DIRECTION ( 'NONE',  ( 1.000000000000000000, 0.000000000000000000, -0.000000000000000000 ) ) ;
#347 = CARTESIAN_POINT ( 'NONE',  ( -20.36124356129798940, 129.6266993258962259, -15.48147584998389448 ) ) ;
#348 = DIRECTION ( 'NONE',  ( -0.000000000000000000, -1.000000000000000000, -0.000000000000000000 ) ) ;
#349 = CARTESIAN_POINT ( 'NONE',  ( -200.0000000000000284, -62.36067977499792647, -25.00000000000000000 ) ) ;
#350 = PLANE ( 'NONE',  #14058 ) ;
#351 = ORIENTED_EDGE ( 'NONE', *, *, #20821, .F. ) ;
#352 = CARTESIAN_POINT ( 'NONE',  ( 343.6424681707624700, 87.16319020290713127, -145.0000000000000000 ) ) ;
#353 = LINE ( 'NONE', #9111, #26676 ) ;
#354 = CARTESIAN_POINT ( 'NONE',  ( 158.0000000000009095, 118.6849996997183041, -45.00000000000000000 ) ) ;
#355 = CARTESIAN_POINT ( 'NONE',  ( 158.0000000000011937, 91.09837461714084839, 45.00000000000000000 ) ) ;
#356 = AXIS2_PLACEMENT_3D ( 'NONE', #3713, #19096, #27838 ) ;
#357 = ORIENTED_EDGE ( 'NONE', *, *, #17681, .T. ) ;
#358 = CARTESIAN_POINT ( 'NONE',  ( 157.4999999999998579, 75.79718706834503905, -45.00000000000000000 ) ) ;
#359 = ORIENTED_EDGE ( 'NONE', *, *, #19187, .F. ) ;
#360 = LINE ( 'NONE', #2786, #27655 ) ;
#361 = CARTESIAN_POINT ( 'NONE',  ( -212.8228108689317253, 60.01962377528476367, -15.18702394368705910 ) ) ;
#362 = DIRECTION ( 'NONE',  ( -0.000000000000000000, -0.000000000000000000, 1.000000000000000000 ) ) ;
#363 = ORIENTED_EDGE ( 'NONE', *, *, #1797, .T. ) ;
#364 = DIRECTION ( 'NONE',  ( -0.000000000000000000, -0.000000000000000000, -1.000000000000000000 ) ) ;
#365 = PRESENTATION_STYLE_ASSIGNMENT (( #221 ) ) ;
#366 = VERTEX_POINT ( 'NONE', #3605 ) ;
#367 = CARTESIAN_POINT ( 'NONE',  ( 158.0000000000009948, 110.6534996696901345, 45.00000000000000000 ) ) ;
#368 = ORIENTED_EDGE ( 'NONE', *, *, #18128, .T. ) ;
#369 = DIRECTION ( 'NONE',  ( 0.4528218681382713551, -0.8916010070293584056, 0.000000000000000000 ) ) ;
#370 = ORIENTED_EDGE ( 'NONE', *, *, #13729, .T. ) ;
#371 = EDGE_CURVE ( 'NONE', #22058, #17465, #16421, .T. ) ;
#372 = VERTEX_POINT ( 'NONE', #14405 ) ;
#373 = DIRECTION ( 'NONE',  ( 1.000000000000000000, 0.000000000000000000, 0.000000000000000000 ) ) ;
#374 = ORIENTED_EDGE ( 'NONE', *, *, #24300, .F. ) ;
#375 = VECTOR ( 'NONE', #26131, 1000.000000000000000 ) ;
#376 = EDGE_CURVE ( 'NONE', #12778, #5204, #20994, .T. ) ;
#377 = AXIS2_PLACEMENT_3D ( 'NONE', #16713, #14560, #19139 ) ;
#378 = VERTEX_POINT ( 'NONE', #12116 ) ;
#379 = ORIENTED_EDGE ( 'NONE', *, *, #16079, .F. ) ;
#380 = CARTESIAN_POINT ( 'NONE',  ( 93.89426149341781525, 239.9406732612975475, 18.26413231115399682 ) ) ;
#381 = CARTESIAN_POINT ( 'NONE',  ( 502.4999999999996021, 44.41075299063184190, 75.35061095560295996 ) ) ;
#382 = DIRECTION ( 'NONE',  ( 0.4528218681372921939, 0.8916010070298556744, -0.000000000000000000 ) ) ;
#383 = DIRECTION ( 'NONE',  ( 0.000000000000000000, 0.000000000000000000, 1.000000000000000000 ) ) ;
#384 = DIRECTION ( 'NONE',  ( -0.000000000000000000, -0.000000000000000000, -1.000000000000000000 ) ) ;
#385 = DIRECTION ( 'NONE',  ( 0.000000000000000000, 0.000000000000000000, 1.000000000000000000 ) ) ;
#386 = EDGE_CURVE ( 'NONE', #7620, #226, #11835, .T. ) ;
#387 = VECTOR ( 'NONE', #7151, 1000.000000000000000 ) ;
#388 = CARTESIAN_POINT ( 'NONE',  ( 1.250275373174978277, -1.249999999999998890, -7.480737022738205511 ) ) ;
#389 = LINE ( 'NONE', #22364, #14037 ) ;
#390 = CARTESIAN_POINT ( 'NONE',  ( 158.0000000000001990, 188.3976249024084666, 45.00000000000000000 ) ) ;
#391 = LINE ( 'NONE', #13469, #619 ) ;
#392 = EDGE_LOOP ( 'NONE', ( #28228, #13403, #15144, #3135 ) ) ;
#393 = DIRECTION ( 'NONE',  ( -0.8498245983676009363, -0.3891357156574876686, 0.3554877590144011057 ) ) ;
#394 = AXIS2_PLACEMENT_3D ( 'NONE', #22078, #2964, #5263 ) ;
#395 = AXIS2_PLACEMENT_3D ( 'NONE', #17054, #6519, #15304 ) ;
#396 = CARTESIAN_POINT ( 'NONE',  ( 232.4999999999996305, 494.4107529906318632, 75.35061095560301681 ) ) ;
#397 = DIRECTION ( 'NONE',  ( -0.8916010070293711731, 0.4528218681382463751, 0.000000000000000000 ) ) ;
#398 = CARTESIAN_POINT ( 'NONE',  ( 106.7495716636776137, 209.9043484200207388, -142.3407963099403446 ) ) ;
#399 = ORIENTED_EDGE ( 'NONE', *, *, #10312, .F. ) ;
#400 = EDGE_CURVE ( 'NONE', #4420, #2951, #20623, .T. ) ;
#401 = DIRECTION ( 'NONE',  ( 0.000000000000000000, 0.000000000000000000, -1.000000000000000000 ) ) ;
#402 = ORIENTED_EDGE ( 'NONE', *, *, #11663, .T. ) ;
#403 = CARTESIAN_POINT ( 'NONE',  ( 232.4999999999996305, 494.4107529906318632, -75.35061095560287470 ) ) ;
#404 = ORIENTED_EDGE ( 'NONE', *, *, #19852, .F. ) ;
#405 = ORIENTED_EDGE ( 'NONE', *, *, #27601, .F. ) ;
#406 = EDGE_CURVE ( 'NONE', #3986, #26642, #16284, .T. ) ;
#407 = VECTOR ( 'NONE', #3303, 1000.000000000000000 ) ;
#408 = EDGE_LOOP ( 'NONE', ( #9219, #25469, #5579, #24964 ) ) ;
#409 = ORIENTED_EDGE ( 'NONE', *, *, #12, .F. ) ;
#410 = VERTEX_POINT ( 'NONE', #9531 ) ;
#411 = ORIENTED_EDGE ( 'NONE', *, *, #8546, .F. ) ;
#412 = PLANE ( 'NONE',  #4933 ) ;
#413 = LINE ( 'NONE', #26684, #6547 ) ;
#414 = VECTOR ( 'NONE', #24913, 999.9999999999998863 ) ;
#415 = AXIS2_PLACEMENT_3D ( 'NONE', #13536, #20551, #20125 ) ;
#416 = CYLINDRICAL_SURFACE ( 'NONE', #20614, 5.000000000000004441 ) ;
#417 = CARTESIAN_POINT ( 'NONE',  ( -8.428214953819216149, 132.5195342171013806, 14.39912748063941983 ) ) ;
#418 = EDGE_CURVE ( 'NONE', #905, #12668, #18291, .T. ) ;
#419 = CARTESIAN_POINT ( 'NONE',  ( -217.7467898461135576, 60.55642267084821384, 12.19614748119721703 ) ) ;
#420 = DIRECTION ( 'NONE',  ( 1.000000000000000000, 0.000000000000000000, 0.000000000000000000 ) ) ;
#421 = PLANE ( 'NONE',  #16345 ) ;
#422 = EDGE_CURVE ( 'NONE', #9422, #12999, #20714, .T. ) ;
#423 = CARTESIAN_POINT ( 'NONE',  ( 158.0000000000015348, 58.49599951954928656, -45.00000000000000000 ) ) ;
#424 = CARTESIAN_POINT ( 'NONE',  ( 158.0000000000016485, 48.46449948952110987, -45.00000000000000000 ) ) ;
#425 = CARTESIAN_POINT ( 'NONE',  ( -42.99650729631200363, 71.03850157808263077, 100.0000000000000000 ) ) ;
#426 = CARTESIAN_POINT ( 'NONE',  ( 119.4436508138959567, 203.0294372515225518, 45.00000000000000000 ) ) ;
#427 = CARTESIAN_POINT ( 'NONE',  ( 0.3999999999999999667, 0.000000000000000000, 0.000000000000000000 ) ) ;
#429 = CARTESIAN_POINT ( 'NONE',  ( 8.117852850209660076, 141.5785587194356481, 12.99999999999999467 ) ) ;
#428 = AXIS2_PLACEMENT_3D ( 'NONE', #23182, #1479, #8092 ) ;
#430 = CARTESIAN_POINT ( 'NONE',  ( 109.9999999999999005, 260.0000000000000000, 45.00000000000000000 ) ) ;
#431 = AXIS2_PLACEMENT_3D ( 'NONE', #7930, #14686, #18707 ) ;
#432 = CARTESIAN_POINT ( 'NONE',  ( 158.0000000000015632, 57.98812451204224061, 45.00000000000000000 ) ) ;
#433 = CARTESIAN_POINT ( 'NONE',  ( -210.0000000000000568, -150.0000000000000853, 110.0000000000000284 ) ) ;
#435 = EDGE_LOOP ( 'NONE', ( #624, #23156, #10826, #824 ) ) ;
#434 = ORIENTED_EDGE ( 'NONE', *, *, #7614, .T. ) ;
#436 = EDGE_CURVE ( 'NONE', #9697, #410, #7928, .T. ) ;
#437 = DIRECTION ( 'NONE',  ( -0.000000000000000000, 0.000000000000000000, -1.000000000000000000 ) ) ;
#438 = VECTOR ( 'NONE', #7033, 1000.000000000000000 ) ;
#439 = CARTESIAN_POINT ( 'NONE',  ( -175.0000000000000000, -120.0250000000001904, -76.00000000000000000 ) ) ;
#440 = CARTESIAN_POINT ( 'NONE',  ( -203.3278902001933659, 92.92226908766613747, -29.32321494459340627 ) ) ;
#441 = ORIENTED_EDGE ( 'NONE', *, *, #25815, .T. ) ;
#442 = ORIENTED_EDGE ( 'NONE', *, *, #67, .F. ) ;
#443 = ADVANCED_FACE ( 'NONE', ( #16699 ), #5898, .T. ) ;
#445 = EDGE_CURVE ( 'NONE', #15077, #27477, #22877, .T. ) ;
#444 = ORIENTED_EDGE ( 'NONE', *, *, #19204, .F. ) ;
#446 = CYLINDRICAL_SURFACE ( 'NONE', #26258, 30.00000000000000000 ) ;
#447 = EDGE_LOOP ( 'NONE', ( #17565, #15243, #25837, #22811 ) ) ;
#448 = EDGE_CURVE ( 'NONE', #7332, #22290, #1039, .T. ) ;
#449 = ORIENTED_EDGE ( 'NONE', *, *, #2534, .F. ) ;
#450 = LINE ( 'NONE', #307, #16398 ) ;
#451 = CIRCLE ( 'NONE', #6855, 5.000000000000000000 ) ;
#452 = DIRECTION ( 'NONE',  ( -0.000000000000000000, -1.000000000000000000, -0.000000000000000000 ) ) ;
#453 = ORIENTED_EDGE ( 'NONE', *, *, #4349, .T. ) ;
#454 = DIRECTION ( 'NONE',  ( 0.000000000000000000, -1.000000000000000000, 0.000000000000000000 ) ) ;
#455 = LINE ( 'NONE', #4177, #5667 ) ;
#456 = VECTOR ( 'NONE', #13195, 1000.000000000000000 ) ;
#457 = CARTESIAN_POINT ( 'NONE',  ( 319.9779125536060178, 113.2029523930392969, -145.0000000000000000 ) ) ;
#458 = LINE ( 'NONE', #9217, #23812 ) ;
#459 = CARTESIAN_POINT ( 'NONE',  ( -213.5622695550096353, 60.06483686772719466, -14.69413405016890017 ) ) ;
#460 = ORIENTED_EDGE ( 'NONE', *, *, #16342, .F. ) ;
#461 = DIRECTION ( 'NONE',  ( 1.000000000000000000, 0.000000000000000000, -0.000000000000000000 ) ) ;
#462 = CARTESIAN_POINT ( 'NONE',  ( -224.0127348693990257, 134.1242697789267027, -15.11921763785539774 ) ) ;
#463 = CARTESIAN_POINT ( 'NONE',  ( 267.4999999999996021, 194.4107529906317779, -100.0000000000000000 ) ) ;
#464 = CARTESIAN_POINT ( 'NONE',  ( 158.0000000000012790, 83.57474959461971764, -45.00000000000000000 ) ) ;
#465 = VERTEX_POINT ( 'NONE', #23870 ) ;
#466 = DIRECTION ( 'NONE',  ( 1.000000000000000000, -0.000000000000000000, 0.000000000000000000 ) ) ;
#467 = VECTOR ( 'NONE', #25215, 1000.000000000000000 ) ;
#468 = CARTESIAN_POINT ( 'NONE',  ( 157.6866818850739662, 8.471341669691319964, -45.00000000000000000 ) ) ;
#469 = LINE ( 'NONE', #26317, #19493 ) ;
#470 = ORIENTED_EDGE ( 'NONE', *, *, #18887, .F. ) ;
#471 = ORIENTED_EDGE ( 'NONE', *, *, #8870, .T. ) ;
#472 = ADVANCED_FACE ( 'NONE', ( #8071 ), #26010, .F. ) ;
#473 = ADVANCED_FACE ( 'NONE', ( #3894 ), #19413, .T. ) ;
#474 = VECTOR ( 'NONE', #16394, 1000.000000000000000 ) ;
#475 = DIRECTION ( 'NONE',  ( 0.2066290158914539099, -0.9784193629480814058, 0.000000000000000000 ) ) ;
#476 = DIRECTION ( 'NONE',  ( -1.000000000000000000, -9.251858538542961967E-16, 0.000000000000000000 ) ) ;
#477 = VERTEX_POINT ( 'NONE', #6332 ) ;
#478 = ORIENTED_EDGE ( 'NONE', *, *, #3698, .F. ) ;
#479 = DIRECTION ( 'NONE',  ( -0.8916010070298252543, 0.4528218681373520904, 0.000000000000000000 ) ) ;
#480 = FACE_OUTER_BOUND ( 'NONE', #21815, .T. ) ;
#481 = ORIENTED_EDGE ( 'NONE', *, *, #25209, .F. ) ;
#482 = CARTESIAN_POINT ( 'NONE',  ( 157.4999999999998579, 63.25781203080982351, 45.00000000000000000 ) ) ;
#483 = ORIENTED_EDGE ( 'NONE', *, *, #21141, .F. ) ;
#484 = CARTESIAN_POINT ( 'NONE',  ( -40.77925748874363165, 129.1862645484492020, 17.01096724815181460 ) ) ;
#485 = VECTOR ( 'NONE', #5220, 999.9999999999998863 ) ;
#486 = EDGE_CURVE ( 'NONE', #2468, #22451, #19269, .T. ) ;
#487 = CARTESIAN_POINT ( 'NONE',  ( 158.0000000000007390, 135.7322497447605656, -45.00000000000000000 ) ) ;
#488 = DIRECTION ( 'NONE',  ( 1.000000000000000000, -0.000000000000000000, 0.000000000000000000 ) ) ;
#489 = CARTESIAN_POINT ( 'NONE',  ( 8.117852850209603233, 141.5785587194356197, -15.00000000000000000 ) ) ;
#490 = DIRECTION ( 'NONE',  ( -1.000000000000000000, 0.000000000000000000, 0.000000000000000000 ) ) ;
#491 = CARTESIAN_POINT ( 'NONE',  ( -270.0517793156885205, -165.1952670567707173, -88.29534001765418338 ) ) ;
#492 = CIRCLE ( 'NONE', #5533, 1.999999999999996669 ) ;
#493 = FACE_OUTER_BOUND ( 'NONE', #792, .T. ) ;
#494 = ORIENTED_EDGE ( 'NONE', *, *, #19922, .T. ) ;
#495 = EDGE_CURVE ( 'NONE', #465, #26764, #24012, .T. ) ;
#496 = DIRECTION ( 'NONE',  ( 0.000000000000000000, -1.000000000000000000, -1.214306433183764966E-16 ) ) ;
#497 = DIRECTION ( 'NONE',  ( -0.8916010070293783896, -0.4528218681382319422, 0.000000000000000000 ) ) ;
#498 = DIRECTION ( 'NONE',  ( 1.000000000000000000, -0.000000000000000000, -0.000000000000000000 ) ) ;
#499 = DIRECTION ( 'NONE',  ( 0.000000000000000000, 0.000000000000000000, -1.000000000000000000 ) ) ;
#500 = ORIENTED_EDGE ( 'NONE', *, *, #25165, .F. ) ;
#501 = LINE ( 'NONE', #24916, #3156 ) ;
#502 = VERTEX_POINT ( 'NONE', #8357 ) ;
#503 = DIRECTION ( 'NONE',  ( -0.000000000000000000, -0.000000000000000000, -1.000000000000000000 ) ) ;
#504 = FACE_OUTER_BOUND ( 'NONE', #21590, .T. ) ;
#505 = CARTESIAN_POINT ( 'NONE',  ( 135.3975132654479125, 250.0000000000000568, -151.0000000000000568 ) ) ;
#506 = VERTEX_POINT ( 'NONE', #21563 ) ;
#507 = CARTESIAN_POINT ( 'NONE',  ( 158.0000000000009663, 113.1613746771971876, 45.00000000000000000 ) ) ;
#508 = EDGE_CURVE ( 'NONE', #26994, #8764, #18328, .T. ) ;
#509 = ORIENTED_EDGE ( 'NONE', *, *, #9465, .F. ) ;
#510 = ADVANCED_FACE ( 'NONE', ( #1873 ), #18986, .F. ) ;
#511 = COLOUR_RGB ( '',0.7921568627450980005, 0.8196078431372548767, 0.9333333333333333481 ) ;
#512 = CARTESIAN_POINT ( 'NONE',  ( -207.5836773499184176, 75.53976764568116664, 42.88623166414009091 ) ) ;
#513 = EDGE_LOOP ( 'NONE', ( #20470, #9702, #23689, #21030 ) ) ;
#514 = EDGE_CURVE ( 'NONE', #16325, #12071, #12961, .T. ) ;
#515 = CARTESIAN_POINT ( 'NONE',  ( -263.9103269956589770, -171.2705086194569901, -104.9999999999999005 ) ) ;
#516 = ORIENTED_EDGE ( 'NONE', *, *, #371, .F. ) ;
#517 = ORIENTED_EDGE ( 'NONE', *, *, #21468, .T. ) ;
#518 = PLANE ( 'NONE',  #26438 ) ;
#519 = ORIENTED_EDGE ( 'NONE', *, *, #2998, .T. ) ;
#520 = VECTOR ( 'NONE', #1855, 1000.000000000000000 ) ;
#521 = ORIENTED_EDGE ( 'NONE', *, *, #18351, .F. ) ;
#522 = EDGE_LOOP ( 'NONE', ( #13816, #10578, #2122, #14859 ) ) ;
#523 = CARTESIAN_POINT ( 'NONE',  ( 94.98941689213133088, 231.7050943134730687, 19.00901305069102065 ) ) ;
#524 = LINE ( 'NONE', #27357, #13105 ) ;
#525 = CARTESIAN_POINT ( 'NONE',  ( 113.4538925329242574, 207.5603490538955782, -145.0000000000000000 ) ) ;
#526 = CARTESIAN_POINT ( 'NONE',  ( 158.0000000000002274, 183.8897498949014278, 45.00000000000000000 ) ) ;
#527 = CARTESIAN_POINT ( 'NONE',  ( -110.3221550338875687, 20.24192588826928585, 83.00000000000001421 ) ) ;
#528 = CYLINDRICAL_SURFACE ( 'NONE', #15262, 22.49999999999999289 ) ;
#529 = TOROIDAL_SURFACE ( 'NONE', #23467, 19.29759039828519818, 4.355764593064427537 ) ;
#530 = CARTESIAN_POINT ( 'NONE',  ( -190.0000000000000284, 59.99999999999995026, 110.0000000000000284 ) ) ;
#531 = CARTESIAN_POINT ( 'NONE',  ( 167.4999999999996589, -5.589247009368137675, -74.99999999999995737 ) ) ;
#532 = CARTESIAN_POINT ( 'NONE',  ( 157.4999999999998579, 105.8916871584295478, -45.00000000000000000 ) ) ;
#533 = CARTESIAN_POINT ( 'NONE',  ( 22.58950924271104554, 154.2349915562422780, 12.99999999999999822 ) ) ;
#534 = LINE ( 'NONE', #11755, #24010 ) ;
#535 = COLOUR_RGB ( '',0.7921568627450980005, 0.8196078431372548767, 0.9333333333333333481 ) ;
#536 = ORIENTED_EDGE ( 'NONE', *, *, #7121, .T. ) ;
#537 = CARTESIAN_POINT ( 'NONE',  ( 157.4999999999998010, 241.3169375638095460, -45.00000000000000000 ) ) ;
#538 = CIRCLE ( 'NONE', #24856, 60.90601976618767566 ) ;
#539 = ADVANCED_FACE ( 'NONE', ( #26156 ), #27734, .T. ) ;
#540 = CARTESIAN_POINT ( 'NONE',  ( 157.4999999999998579, 191.1594374136689964, -45.00000000000000000 ) ) ;
#541 = CARTESIAN_POINT ( 'NONE',  ( 139.9999999999999716, -120.0000000000000995, 100.0000000000000142 ) ) ;
#542 = PLANE ( 'NONE',  #20720 ) ;
#543 = VERTEX_POINT ( 'NONE', #17395 ) ;
#544 = CARTESIAN_POINT ( 'NONE',  ( 108.8501248000116277, 253.0299650808884735, -36.51570041470898076 ) ) ;
#545 = ORIENTED_EDGE ( 'NONE', *, *, #17891, .F. ) ;
#546 = EDGE_CURVE ( 'NONE', #991, #20740, #6197, .T. ) ;
#547 = CARTESIAN_POINT ( 'NONE',  ( 157.4999999999998579, 153.5413123010633853, 45.00000000000000000 ) ) ;
#548 = VERTEX_POINT ( 'NONE', #21136 ) ;
#549 = EDGE_CURVE ( 'NONE', #10475, #4407, #3984, .T. ) ;
#550 = VECTOR ( 'NONE', #13292, 1000.000000000000114 ) ;
#551 = ORIENTED_EDGE ( 'NONE', *, *, #12670, .T. ) ;
#552 = ORIENTED_EDGE ( 'NONE', *, *, #17681, .F. ) ;
#553 = VERTEX_POINT ( 'NONE', #7053 ) ;
#554 = VECTOR ( 'NONE', #22307, 1000.000000000000000 ) ;
#555 = CARTESIAN_POINT ( 'NONE',  ( -92.89766067256680060, 136.4115285999503158, 13.49165197499294599 ) ) ;
#556 = DIRECTION ( 'NONE',  ( 1.000000000000000000, 0.000000000000000000, 0.000000000000000000 ) ) ;
#557 = DIRECTION ( 'NONE',  ( -0.9659258262890705327, -0.2588190451025121908, 0.000000000000000000 ) ) ;
#558 = VECTOR ( 'NONE', #22339, 1000.000000000000000 ) ;
#559 = CARTESIAN_POINT ( 'NONE',  ( -97.83215868775270962, 136.0971436861518669, -15.20870553203125120 ) ) ;
#560 = PRODUCT_DEFINITION_CONTEXT ( 'detailed design', #11879, 'design' ) ;
#561 = CARTESIAN_POINT ( 'NONE',  ( 155.4185842870419947, 230.6339745962152392, -45.00000000000000000 ) ) ;
#562 = CARTESIAN_POINT ( 'NONE',  ( -218.4636426211929177, 60.67881959240470735, 11.81164476506740790 ) ) ;
#563 = CARTESIAN_POINT ( 'NONE',  ( 157.9999999999996874, 268.6496251426330559, -45.00000000000000000 ) ) ;
#564 = LINE ( 'NONE', #17941, #18623 ) ;
#565 = DIRECTION ( 'NONE',  ( 0.5975062131282562472, -0.8018642810807392607, 0.000000000000000000 ) ) ;
#566 = CARTESIAN_POINT ( 'NONE',  ( -229.8938360676123978, 91.85985842061924700, -13.11794914285764690 ) ) ;
#567 = DIRECTION ( 'NONE',  ( -0.8142945039115421224, -0.5804519453834706688, 0.000000000000000000 ) ) ;
#568 = DIRECTION ( 'NONE',  ( 1.000000000000000000, -0.000000000000000000, -0.000000000000000000 ) ) ;
#569 = CARTESIAN_POINT ( 'NONE',  ( 157.9999999999998010, 238.5551250525490161, 45.00000000000000000 ) ) ;
#570 = EDGE_CURVE ( 'NONE', #7917, #3329, #15402, .T. ) ;
#571 = VECTOR ( 'NONE', #26169, 1000.000000000000227 ) ;
#572 = CARTESIAN_POINT ( 'NONE',  ( -18.11108351247773385, 129.9683555792950358, 15.33266781369627907 ) ) ;
#573 = CARTESIAN_POINT ( 'NONE',  ( 232.4999999999996305, 44.41075299063184190, 75.35061095560295996 ) ) ;
#574 = CARTESIAN_POINT ( 'NONE',  ( 158.0000000000013358, 78.55899957960562574, -45.00000000000000000 ) ) ;
#575 = CARTESIAN_POINT ( 'NONE',  ( -107.3221550338875687, 17.24192588826928585, 83.00000000000001421 ) ) ;
#576 = AXIS2_PLACEMENT_3D ( 'NONE', #27144, #7193, #11366 ) ;
#578 = ORIENTED_EDGE ( 'NONE', *, *, #27825, .F. ) ;
#577 = ORIENTED_EDGE ( 'NONE', *, *, #22638, .T. ) ;
#579 = DIRECTION ( 'NONE',  ( -0.8916010070293783896, -0.4528218681382319422, 0.000000000000000000 ) ) ;
#580 = AXIS2_PLACEMENT_3D ( 'NONE', #3424, #12354, #8027 ) ;
#581 = DIRECTION ( 'NONE',  ( 1.000000000000000000, 0.000000000000000000, 0.000000000000000000 ) ) ;
#582 = ORIENTED_EDGE ( 'NONE', *, *, #19199, .T. ) ;
#583 = VERTEX_POINT ( 'NONE', #15541 ) ;
#584 = EDGE_LOOP ( 'NONE', ( #16630, #25625, #9572, #10611, #8685 ) ) ;
#585 = EDGE_CURVE ( 'NONE', #16172, #22496, #15834, .T. ) ;
#586 = CARTESIAN_POINT ( 'NONE',  ( -210.0000000000000568, -157.0000000000000284, -94.99999999999987210 ) ) ;
#587 = EDGE_CURVE ( 'NONE', #6088, #15077, #9133, .T. ) ;
#588 = CARTESIAN_POINT ( 'NONE',  ( 157.9999999999998010, 236.5551250525490161, -45.00000000000000000 ) ) ;
#589 = ORIENTED_EDGE ( 'NONE', *, *, #6265, .F. ) ;
#590 = EDGE_LOOP ( 'NONE', ( #18071, #20954, #25827, #7929 ) ) ;
#591 = CARTESIAN_POINT ( 'NONE',  ( -260.0000000000001137, -167.0819201924624906, -109.9999999999998721 ) ) ;
#592 = AXIS2_PLACEMENT_3D ( 'NONE', #13930, #17784, #13641 ) ;
#593 = DIRECTION ( 'NONE',  ( 0.000000000000000000, 0.000000000000000000, -1.000000000000000000 ) ) ;
#594 = AXIS2_PLACEMENT_3D ( 'NONE', #26284, #2003, #28279 ) ;
#595 = DIRECTION ( 'NONE',  ( 0.000000000000000000, 0.000000000000000000, 1.000000000000000000 ) ) ;
#596 = ORIENTED_EDGE ( 'NONE', *, *, #20943, .T. ) ;
#597 = CARTESIAN_POINT ( 'NONE',  ( -205.5646887631684763, 90.70208198090838891, 28.50398098557788273 ) ) ;
#598 = CIRCLE ( 'NONE', #1034, 7.499999999999992895 ) ;
#599 = LINE ( 'NONE', #25008, #4734 ) ;
#600 = EDGE_CURVE ( 'NONE', #17042, #11042, #25180, .T. ) ;
#601 = VECTOR ( 'NONE', #28078, 1000.000000000000000 ) ;
#602 = EDGE_CURVE ( 'NONE', #11526, #18196, #21990, .T. ) ;
#603 = CARTESIAN_POINT ( 'NONE',  ( 134.9999999999998579, 220.0000000000000284, -119.9999999999999858 ) ) ;
#604 = CARTESIAN_POINT ( 'NONE',  ( 109.9999999999999005, 240.0000000000000284, 15.00000000000000000 ) ) ;
#605 = CARTESIAN_POINT ( 'NONE',  ( -214.3579997887104298, 72.01340221155322752, -27.44224251620622113 ) ) ;
#606 = VERTEX_POINT ( 'NONE', #11525 ) ;
#607 = CARTESIAN_POINT ( 'NONE',  ( 217.4999999999996305, 133.0668745871126930, 36.86484227207694886 ) ) ;
#608 = EDGE_CURVE ( 'NONE', #5724, #21166, #15684, .T. ) ;
#609 = DIRECTION ( 'NONE',  ( -0.8379557447115514313, 0.5457381880580733924, 0.000000000000000000 ) ) ;
#610 = CARTESIAN_POINT ( 'NONE',  ( 187.4999999999996305, 258.6181251126050711, 1.387778780781445676E-14 ) ) ;
#611 = CARTESIAN_POINT ( 'NONE',  ( -200.0000000000000284, 0.000000000000000000, -25.00000000000000000 ) ) ;
#612 = ORIENTED_EDGE ( 'NONE', *, *, #27121, .T. ) ;
#613 = AXIS2_PLACEMENT_3D ( 'NONE', #4215, #27908, #25767 ) ;
#614 = CARTESIAN_POINT ( 'NONE',  ( 46.79174272583949801, 194.0572550123460474, 12.99999999999999822 ) ) ;
#615 = VECTOR ( 'NONE', #20884, 1000.000000000000114 ) ;
#616 = FACE_OUTER_BOUND ( 'NONE', #8502, .T. ) ;
#617 = LINE ( 'NONE', #13264, #2052 ) ;
#618 = ORIENTED_EDGE ( 'NONE', *, *, #5223, .T. ) ;
#619 = VECTOR ( 'NONE', #22222, 1000.000000000000000 ) ;
#620 = VERTEX_POINT ( 'NONE', #11079 ) ;
#621 = CARTESIAN_POINT ( 'NONE',  ( 81.45493510940914916, 110.0000000000000142, 70.00000000030220804 ) ) ;
#622 = CARTESIAN_POINT ( 'NONE',  ( -266.5839533485339530, -91.18033988749901653, -15.26911010665567225 ) ) ;
#623 = ORIENTED_EDGE ( 'NONE', *, *, #7231, .T. ) ;
#624 = ORIENTED_EDGE ( 'NONE', *, *, #701, .T. ) ;
#625 = CARTESIAN_POINT ( 'NONE',  ( 134.9999999999998579, 220.0000000000000284, 99.00000000000001421 ) ) ;
#626 = CARTESIAN_POINT ( 'NONE',  ( 0.000000000000000000, 0.000000000000000000, 45.00000000000000000 ) ) ;
#627 = VERTEX_POINT ( 'NONE', #26725 ) ;
#628 = DIRECTION ( 'NONE',  ( 0.4528218681370924092, 0.8916010070299572599, -0.000000000000000000 ) ) ;
#629 = ORIENTED_EDGE ( 'NONE', *, *, #2343, .F. ) ;
#630 = AXIS2_PLACEMENT_3D ( 'NONE', #3020, #873, #5034 ) ;
#631 = LINE ( 'NONE', #7377, #27214 ) ;
#632 = VECTOR ( 'NONE', #24895, 1000.000000000000000 ) ;
#633 = DIRECTION ( 'NONE',  ( 1.000000000000000000, 0.000000000000000000, -0.000000000000000000 ) ) ;
#634 = DIRECTION ( 'NONE',  ( 0.000000000000000000, 0.000000000000000000, -1.000000000000000000 ) ) ;
#635 = CARTESIAN_POINT ( 'NONE',  ( 0.6797495551325769547, 136.5999822166548370, -13.39362083918624968 ) ) ;
#636 = CONICAL_SURFACE ( 'NONE', #13495, 5.999999999999977796, 1.029744258676652091 ) ;
#637 = DIRECTION ( 'NONE',  ( -0.000000000000000000, -0.000000000000000000, 1.000000000000000000 ) ) ;
#638 = ADVANCED_FACE ( 'NONE', ( #4745 ), #27027, .F. ) ;
#639 = CARTESIAN_POINT ( 'NONE',  ( 179.9999999999999147, -150.0000000000000284, 84.99999999999995737 ) ) ;
#640 = CARTESIAN_POINT ( 'NONE',  ( 162.1315766072936242, 207.1972522101084735, -139.5322470298331439 ) ) ;
#641 = ORIENTED_EDGE ( 'NONE', *, *, #2045, .T. ) ;
#642 = LINE ( 'NONE', #11850, #26984 ) ;
#643 = CARTESIAN_POINT ( 'NONE',  ( 158.0000000000003126, 176.3661248723802828, 45.00000000000000000 ) ) ;
#644 = DIRECTION ( 'NONE',  ( -0.000000000000000000, -0.000000000000000000, -1.000000000000000000 ) ) ;
#645 = DIRECTION ( 'NONE',  ( -0.000000000000000000, 1.000000000000000000, -1.387778780781445429E-16 ) ) ;
#646 = ORIENTED_EDGE ( 'NONE', *, *, #18826, .T. ) ;
#647 = DIRECTION ( 'NONE',  ( 0.5555587585212683477, 0.8314772792026894344, -0.000000000000000000 ) ) ;
#648 = ORIENTED_EDGE ( 'NONE', *, *, #18190, .T. ) ;
#649 = LINE ( 'NONE', #27065, #16667 ) ;
#650 = LINE ( 'NONE', #20465, #20665 ) ;
#651 = CARTESIAN_POINT ( 'NONE',  ( 138.1747091788253954, 249.8319942030928758, -139.9049692442122534 ) ) ;
#652 = ORIENTED_EDGE ( 'NONE', *, *, #23081, .T. ) ;
#653 = CARTESIAN_POINT ( 'NONE',  ( 109.9999999999999005, 260.0000000000000000, 45.00000000000000000 ) ) ;
#654 = ORIENTED_EDGE ( 'NONE', *, *, #6112, .T. ) ;
#655 = VECTOR ( 'NONE', #25630, 1000.000000000000000 ) ;
#656 = FACE_OUTER_BOUND ( 'NONE', #25895, .T. ) ;
#657 = ORIENTED_EDGE ( 'NONE', *, *, #26807, .T. ) ;
#658 = CARTESIAN_POINT ( 'NONE',  ( 91.94652509811839991, 240.0740392588532757, 7.116191647120904129 ) ) ;
#659 = ORIENTED_EDGE ( 'NONE', *, *, #1539, .T. ) ;
#660 = VECTOR ( 'NONE', #1060, 1000.000000000000114 ) ;
#661 = ORIENTED_EDGE ( 'NONE', *, *, #5035, .T. ) ;
#662 = DIRECTION ( 'NONE',  ( 0.000000000000000000, 1.214306433183764966E-16, -1.000000000000000000 ) ) ;
#663 = ORIENTED_EDGE ( 'NONE', *, *, #22607, .F. ) ;
#664 = EDGE_CURVE ( 'NONE', #22382, #5522, #13383, .T. ) ;
#665 = EDGE_LOOP ( 'NONE', ( #21, #21281, #16990, #8206, #12330, #23398, #10718, #5703 ) ) ;
#666 = ORIENTED_EDGE ( 'NONE', *, *, #14204, .T. ) ;
#667 = CARTESIAN_POINT ( 'NONE',  ( 101.4665947576538372, 243.5985648160911410, 15.64809332289330435 ) ) ;
#668 =( REPRESENTATION_RELATIONSHIP ('NONE','NONE', #11963, #3128 ) REPRESENTATION_RELATIONSHIP_WITH_TRANSFORMATION ( #3881 )SHAPE_REPRESENTATION_RELATIONSHIP( ) );
#669 = DIRECTION ( 'NONE',  ( 0.000000000000000000, 0.000000000000000000, 1.000000000000000000 ) ) ;
#670 = EDGE_CURVE ( 'NONE', #15969, #22271, #11226, .T. ) ;
#671 = CARTESIAN_POINT ( 'NONE',  ( 65.00000000000000000, -150.0000000000000568, -69.99999999999998579 ) ) ;
#672 = CIRCLE ( 'NONE', #14906, 1.999999999999998890 ) ;
#673 = ADVANCED_FACE ( 'NONE', ( #13529 ), #308, .F. ) ;
#674 = EDGE_CURVE ( 'NONE', #21518, #27627, #20135, .T. ) ;
#675 = CARTESIAN_POINT ( 'NONE',  ( 81.45493510941093973, 110.0000000000000142, -70.00000000034538061 ) ) ;
#676 = FACE_OUTER_BOUND ( 'NONE', #18606, .T. ) ;
#677 = FACE_OUTER_BOUND ( 'NONE', #5, .T. ) ;
#678 = EDGE_CURVE ( 'NONE', #16059, #28280, #20119, .T. ) ;
#679 = CARTESIAN_POINT ( 'NONE',  ( 158.0000000000009379, 116.1771246922112653, 45.00000000000000000 ) ) ;
#680 = DIRECTION ( 'NONE',  ( 0.000000000000000000, 0.000000000000000000, -1.000000000000000000 ) ) ;
#681 = CARTESIAN_POINT ( 'NONE',  ( -262.5451564304015619, -171.6056065411685552, 105.0000000000519549 ) ) ;
#682 = DIRECTION ( 'NONE',  ( 1.000000000000000000, 0.000000000000000000, 0.000000000000000000 ) ) ;
#683 = DIRECTION ( 'NONE',  ( 1.000000000000000000, 0.000000000000000000, 0.000000000000000000 ) ) ;
#684 = ORIENTED_EDGE ( 'NONE', *, *, #26881, .T. ) ;
#685 = DIRECTION ( 'NONE',  ( 1.000000000000000000, 0.000000000000000000, -0.000000000000000000 ) ) ;
#686 = CARTESIAN_POINT ( 'NONE',  ( 122.8247714198253959, 235.8670668058242939, 45.00000000000000000 ) ) ;
#687 = CYLINDRICAL_SURFACE ( 'NONE', #19940, 10.00000000000000888 ) ;
#688 = DIRECTION ( 'NONE',  ( 0.000000000000000000, -1.000000000000000000, 0.000000000000000000 ) ) ;
#689 = VERTEX_POINT ( 'NONE', #9212 ) ;
#690 = CARTESIAN_POINT ( 'NONE',  ( -210.0000000000000568, -210.8114316696540982, 110.0000000000000284 ) ) ;
#691 = ORIENTED_EDGE ( 'NONE', *, *, #13967, .F. ) ;
#692 = VECTOR ( 'NONE', #27394, 1000.000000000000114 ) ;
#693 = ORIENTED_EDGE ( 'NONE', *, *, #10754, .F. ) ;
#694 = ORIENTED_EDGE ( 'NONE', *, *, #13779, .T. ) ;
#695 = VERTEX_POINT ( 'NONE', #161 ) ;
#696 = CONICAL_SURFACE ( 'NONE', #16750, 5.999999999999977796, 1.029744258676652979 ) ;
#697 = ORIENTED_EDGE ( 'NONE', *, *, #18565, .F. ) ;
#698 = DIRECTION ( 'NONE',  ( 0.000000000000000000, 0.000000000000000000, -1.000000000000000000 ) ) ;
#699 = DIRECTION ( 'NONE',  ( 0.4528218681376512400, -0.8916010070296733758, 0.000000000000000000 ) ) ;
#700 = CARTESIAN_POINT ( 'NONE',  ( 87.49999999999990052, 230.0000000000000284, 15.95262490344436657 ) ) ;
#701 = EDGE_CURVE ( 'NONE', #9383, #10330, #21856, .T. ) ;
#702 = ADVANCED_FACE ( 'NONE', ( #13675 ), #26432, .T. ) ;
#703 = CARTESIAN_POINT ( 'NONE',  ( -101.5016674773769694, 134.2040548686907755, -15.56499774383584622 ) ) ;
#704 = DIRECTION ( 'NONE',  ( -0.000000000000000000, -0.000000000000000000, -1.000000000000000000 ) ) ;
#705 = CARTESIAN_POINT ( 'NONE',  ( -195.1986077931981356, 62.83738171803135231, 37.97438512083786577 ) ) ;
#706 = CARTESIAN_POINT ( 'NONE',  ( -56.65306767071049165, 63.08575069354419185, 45.00000000000000000 ) ) ;
#707 = CARTESIAN_POINT ( 'NONE',  ( 14.21936997543395798, -49.77566109691134955, 98.36633331184400220 ) ) ;
#708 = EDGE_CURVE ( 'NONE', #12779, #28035, #2160, .T. ) ;
#709 = CARTESIAN_POINT ( 'NONE',  ( 134.6079681791958365, 250.0000000000001137, -138.9999999999999716 ) ) ;
#710 = VECTOR ( 'NONE', #14587, 1000.000000000000000 ) ;
#711 = CARTESIAN_POINT ( 'NONE',  ( 157.4999999999998579, 105.8916871584295478, 45.00000000000000000 ) ) ;
#712 = CARTESIAN_POINT ( 'NONE',  ( 157.4999999999998579, 188.6515624061619576, 45.00000000000000000 ) ) ;
#713 = CARTESIAN_POINT ( 'NONE',  ( 157.4999999999998579, 75.79718706834503905, 45.00000000000000000 ) ) ;
#714 = VECTOR ( 'NONE', #4678, 1000.000000000000000 ) ;
#715 = CARTESIAN_POINT ( 'NONE',  ( 109.9999999999999147, 140.0000000000000000, 90.00000000000002842 ) ) ;
#716 = AXIS2_PLACEMENT_3D ( 'NONE', #20523, #18375, #3692 ) ;
#717 = CARTESIAN_POINT ( 'NONE',  ( 65.00000000000000000, -120.0000000000000711, 70.00000000000001421 ) ) ;
#718 = DIRECTION ( 'NONE',  ( 0.9985600561963489108, -0.05364526231778980747, 0.000000000000000000 ) ) ;
#719 = CARTESIAN_POINT ( 'NONE',  ( 118.4313905927012343, 122.3304618272157569, -100.0000000000000142 ) ) ;
#720 = PLANE ( 'NONE',  #20781 ) ;
#721 = AXIS2_PLACEMENT_3D ( 'NONE', #25156, #27436, #16685 ) ;
#723 = ORIENTED_EDGE ( 'NONE', *, *, #775, .T. ) ;
#722 = ORIENTED_EDGE ( 'NONE', *, *, #6037, .F. ) ;
#724 = CARTESIAN_POINT ( 'NONE',  ( -207.1027104522468392, 89.68341047235171004, -27.43904842249505194 ) ) ;
#725 = ORIENTED_EDGE ( 'NONE', *, *, #13975, .T. ) ;
#726 = ORIENTED_EDGE ( 'NONE', *, *, #26630, .F. ) ;
#727 = FACE_OUTER_BOUND ( 'NONE', #4250, .T. ) ;
#728 = CARTESIAN_POINT ( 'NONE',  ( -144.8818860832173527, 126.6487520769749580, 16.84620022481251311 ) ) ;
#729 = VERTEX_POINT ( 'NONE', #20 ) ;
#730 = ORIENTED_EDGE ( 'NONE', *, *, #11239, .F. ) ;
#731 = CARTESIAN_POINT ( 'NONE',  ( -173.1201715254111662, 113.5802963645813151, -28.20029687320744216 ) ) ;
#732 = VECTOR ( 'NONE', #22180, 1000.000000000000000 ) ;
#733 = VECTOR ( 'NONE', #6685, 1000.000000000000227 ) ;
#734 = CARTESIAN_POINT ( 'NONE',  ( 158.0000000000005400, 156.3031248123239436, 45.00000000000000000 ) ) ;
#735 = EDGE_CURVE ( 'NONE', #14776, #17184, #8778, .T. ) ;
#736 = CARTESIAN_POINT ( 'NONE',  ( 157.9999999999996589, 276.1732501651540588, 45.00000000000000000 ) ) ;
#737 = CARTESIAN_POINT ( 'NONE',  ( -203.3278902001933375, 92.92226908766613747, 29.32321494459339561 ) ) ;
#738 = AXIS2_PLACEMENT_3D ( 'NONE', #16780, #14771, #23524 ) ;
#739 = LINE ( 'NONE', #24727, #13957 ) ;
#740 = CARTESIAN_POINT ( 'NONE',  ( 145.6339745962154097, 240.4185842870418242, 45.00000000000000000 ) ) ;
#741 = LINE ( 'NONE', #5326, #18696 ) ;
#742 = CARTESIAN_POINT ( 'NONE',  ( -213.9337484054510128, 55.48171494544713056, -43.35284082257812344 ) ) ;
#743 = EDGE_CURVE ( 'NONE', #20178, #23548, #16499, .T. ) ;
#744 = ADVANCED_FACE ( 'NONE', ( #5030 ), #27419, .F. ) ;
#745 = LINE ( 'NONE', #26587, #14618 ) ;
#746 = CARTESIAN_POINT ( 'NONE',  ( -227.8378063125350366, 130.6400894613935577, -13.00000000000000178 ) ) ;
#747 = LINE ( 'NONE', #24592, #112 ) ;
#748 = CARTESIAN_POINT ( 'NONE',  ( 157.4999999999998295, 228.7775625262745223, 45.00000000000000000 ) ) ;
#749 = VERTEX_POINT ( 'NONE', #25137 ) ;
#750 = VECTOR ( 'NONE', #15038, 1000.000000000000000 ) ;
#751 = DIRECTION ( 'NONE',  ( -1.000000000000000000, 0.000000000000000000, -0.000000000000000000 ) ) ;
#752 = CARTESIAN_POINT ( 'NONE',  ( -236.2622743973914510, 68.21227378728754331, 5.744226217424930780 ) ) ;
#753 = CARTESIAN_POINT ( 'NONE',  ( 158.0000000000009095, 118.6849996997183041, 45.00000000000000000 ) ) ;
#754 = ORIENTED_EDGE ( 'NONE', *, *, #21243, .F. ) ;
#755 = AXIS2_PLACEMENT_3D ( 'NONE', #22509, #5114, #11751 ) ;
#756 = ORIENTED_EDGE ( 'NONE', *, *, #4498, .T. ) ;
#757 = EDGE_CURVE ( 'NONE', #11653, #6227, #3168, .T. ) ;
#758 = EDGE_CURVE ( 'NONE', #11111, #19970, #7626, .T. ) ;
#759 = LINE ( 'NONE', #16277, #22117 ) ;
#760 = FACE_OUTER_BOUND ( 'NONE', #17355, .T. ) ;
#761 = VERTEX_POINT ( 'NONE', #16391 ) ;
#762 = ORIENTED_EDGE ( 'NONE', *, *, #3865, .T. ) ;
#763 = CARTESIAN_POINT ( 'NONE',  ( -63.57415822541634043, 0.000000000000000000, 95.00000000000000000 ) ) ;
#764 = CARTESIAN_POINT ( 'NONE',  ( -76.25760768171836901, 154.8982798170083299, 12.99999999999999822 ) ) ;
#765 = FACE_OUTER_BOUND ( 'NONE', #3853, .T. ) ;
#766 = ORIENTED_EDGE ( 'NONE', *, *, #9211, .F. ) ;
#767 = FACE_OUTER_BOUND ( 'NONE', #3565, .T. ) ;
#768 = ORIENTED_EDGE ( 'NONE', *, *, #27927, .F. ) ;
#769 = CIRCLE ( 'NONE', #28282, 17.46154499483315448 ) ;
#770 = DIRECTION ( 'NONE',  ( -0.000000000000000000, -0.000000000000000000, 1.000000000000000000 ) ) ;
#771 = CARTESIAN_POINT ( 'NONE',  ( 33.10302365956999182, 219.6666220619077876, -13.00000000000000000 ) ) ;
#772 = DIRECTION ( 'NONE',  ( 1.000000000000000000, 0.000000000000000000, 0.000000000000000000 ) ) ;
#773 = CARTESIAN_POINT ( 'NONE',  ( -7.443950587159290144, 132.8771115358387931, -14.28760955781909381 ) ) ;
#774 = FACE_OUTER_BOUND ( 'NONE', #27445, .T. ) ;
#775 = EDGE_CURVE ( 'NONE', #20816, #23826, #7896, .T. ) ;
#776 = CARTESIAN_POINT ( 'NONE',  ( 232.4999999999996305, 83.06687458711267880, 42.88984227207694033 ) ) ;
#777 = DIRECTION ( 'NONE',  ( 1.000000000000000000, 0.000000000000000000, 0.000000000000000000 ) ) ;
#778 = ORIENTED_EDGE ( 'NONE', *, *, #27716, .F. ) ;
#779 = ADVANCED_FACE ( 'NONE', ( #18261 ), #9781, .T. ) ;
#780 = PLANE ( 'NONE',  #2193 ) ;
#781 = DIRECTION ( 'NONE',  ( 0.7071067811865474617, 0.7071067811865474617, 0.000000000000000000 ) ) ;
#782 = FACE_OUTER_BOUND ( 'NONE', #22813, .T. ) ;
#783 = DIRECTION ( 'NONE',  ( 0.000000000000000000, 0.000000000000000000, -1.000000000000000000 ) ) ;
#784 = EDGE_LOOP ( 'NONE', ( #27213, #18467, #26244, #20332 ) ) ;
#785 = DIRECTION ( 'NONE',  ( 0.000000000000000000, -1.000000000000000000, 0.000000000000000000 ) ) ;
#786 = ORIENTED_EDGE ( 'NONE', *, *, #2510, .F. ) ;
#787 = LINE ( 'NONE', #12142, #8871 ) ;
#788 = PLANE ( 'NONE',  #25217 ) ;
#789 = CARTESIAN_POINT ( 'NONE',  ( 134.9999999999998863, 250.0000000000000568, -151.0000000000000284 ) ) ;
#790 = ORIENTED_EDGE ( 'NONE', *, *, #25750, .F. ) ;
#791 = DIRECTION ( 'NONE',  ( -0.000000000000000000, -0.000000000000000000, -1.000000000000000000 ) ) ;
#792 = EDGE_LOOP ( 'NONE', ( #26456, #9388, #18385, #15458, #18561, #10831 ) ) ;
#793 = VECTOR ( 'NONE', #14680, 1000.000000000000000 ) ;
#794 = EDGE_CURVE ( 'NONE', #15105, #2405, #20829, .T. ) ;
#795 = CIRCLE ( 'NONE', #16840, 9.999999999999994671 ) ;
#796 = FACE_OUTER_BOUND ( 'NONE', #27107, .T. ) ;
#797 = DIRECTION ( 'NONE',  ( 0.000000000000000000, -1.000000000000000000, -1.214306433183764966E-16 ) ) ;
#798 = ORIENTED_EDGE ( 'NONE', *, *, #12480, .F. ) ;
#799 = EDGE_CURVE ( 'NONE', #12071, #26896, #5455, .T. ) ;
#800 = VERTEX_POINT ( 'NONE', #13821 ) ;
#801 = EDGE_CURVE ( 'NONE', #19503, #8160, #22570, .T. ) ;
#802 = DIRECTION ( 'NONE',  ( 0.000000000000000000, 1.000000000000000000, 0.000000000000000000 ) ) ;
#803 = ORIENTED_EDGE ( 'NONE', *, *, #16888, .F. ) ;
#804 = EDGE_CURVE ( 'NONE', #2005, #223, #27933, .T. ) ;
#805 = ORIENTED_EDGE ( 'NONE', *, *, #5908, .F. ) ;
#806 = ORIENTED_EDGE ( 'NONE', *, *, #17778, .T. ) ;
#807 = CARTESIAN_POINT ( 'NONE',  ( 109.9999999999999005, 259.1520133602594456, 44.26562200907745392 ) ) ;
#808 = DIRECTION ( 'NONE',  ( -8.673617379884036705E-17, 1.000000000000000000, 0.000000000000000000 ) ) ;
#809 = LINE ( 'NONE', #11602, #22008 ) ;
#810 = VECTOR ( 'NONE', #4848, 1000.000000000000000 ) ;
#811 = CARTESIAN_POINT ( 'NONE',  ( 85.90765579575543143, 110.5723347142871091, -70.58593750016461854 ) ) ;
#812 = LINE ( 'NONE', #948, #4384 ) ;
#813 = FACE_OUTER_BOUND ( 'NONE', #28354, .T. ) ;
#814 = CARTESIAN_POINT ( 'NONE',  ( 158.0000000000003126, 176.3661248723802828, 45.00000000000000000 ) ) ;
#815 = CARTESIAN_POINT ( 'NONE',  ( 65.00000000000000000, -150.0000000000000568, 70.00000000000001421 ) ) ;
#816 = EDGE_CURVE ( 'NONE', #10360, #6691, #22989, .T. ) ;
#817 = CARTESIAN_POINT ( 'NONE',  ( -267.9882009536668193, -170.6226266830407496, 104.4279108778009828 ) ) ;
#818 = DIRECTION ( 'NONE',  ( 0.8916010070293510781, -0.4528218681382856770, 0.000000000000000000 ) ) ;
#819 = LINE ( 'NONE', #9862, #20338 ) ;
#820 = ORIENTED_EDGE ( 'NONE', *, *, #24259, .F. ) ;
#821 = DIRECTION ( 'NONE',  ( -0.8706753206611566043, -1.365180738000214426E-15, -0.4918581970360891842 ) ) ;
#822 = LINE ( 'NONE', #541, #8481 ) ;
#823 = CARTESIAN_POINT ( 'NONE',  ( -273.6211430000234373, -91.18033988749901653, 0.000000000000000000 ) ) ;
#824 = ORIENTED_EDGE ( 'NONE', *, *, #23421, .T. ) ;
#825 = VECTOR ( 'NONE', #26696, 1000.000000000000000 ) ;
#826 = LINE ( 'NONE', #12322, #17561 ) ;
#827 = ORIENTED_EDGE ( 'NONE', *, *, #20728, .F. ) ;
#828 = CARTESIAN_POINT ( 'NONE',  ( 158.0000000000009095, 118.6849996997183041, -45.00000000000000000 ) ) ;
#829 = ORIENTED_EDGE ( 'NONE', *, *, #22521, .F. ) ;
#830 = EDGE_CURVE ( 'NONE', #12559, #10408, #23836, .T. ) ;
#831 = EDGE_CURVE ( 'NONE', #3911, #16933, #25279, .T. ) ;
#832 = ORIENTED_EDGE ( 'NONE', *, *, #20807, .T. ) ;
#833 = ORIENTED_EDGE ( 'NONE', *, *, #27551, .T. ) ;
#834 = ORIENTED_EDGE ( 'NONE', *, *, #1618, .F. ) ;
#835 = CARTESIAN_POINT ( 'NONE',  ( -151.8667954808881291, 124.0669258736115523, 18.37961917418349955 ) ) ;
#836 = LINE ( 'NONE', #15335, #13752 ) ;
#837 = DIRECTION ( 'NONE',  ( 0.8916010070295106171, -0.4528218681379715393, 0.000000000000000000 ) ) ;
#838 = VECTOR ( 'NONE', #12878, 1000.000000000000000 ) ;
#839 = DIRECTION ( 'NONE',  ( 0.8916010070300181001, -0.4528218681369723941, 0.000000000000000000 ) ) ;
#840 = UNCERTAINTY_MEASURE_WITH_UNIT (LENGTH_MEASURE( 1.000000000000000082E-05 ), #2464, 'distance_accuracy_value', 'NONE');
#841 = CARTESIAN_POINT ( 'NONE',  ( -31.50743868999440167, 129.2243496464543284, 15.65998950894569752 ) ) ;
#842 = CARTESIAN_POINT ( 'NONE',  ( -195.0250397031994112, 62.90385929084195737, 38.63509848415888115 ) ) ;
#844 = CARTESIAN_POINT ( 'NONE',  ( -210.0000000000000000, -218.4793454996983826, 90.61920026979468901 ) ) ;
#843 = AXIS2_PLACEMENT_3D ( 'NONE', #16057, #23075, #9861 ) ;
#845 = DIRECTION ( 'NONE',  ( 0.8916010070293383105, -0.4528218681383106015, 0.000000000000000000 ) ) ;
#846 = CARTESIAN_POINT ( 'NONE',  ( 79.99999999999994316, 109.9999999999999716, -71.96349540849364246 ) ) ;
#847 = VECTOR ( 'NONE', #18718, 1000.000000000000114 ) ;
#848 = CARTESIAN_POINT ( 'NONE',  ( -207.3935809773778942, 90.19561752971078761, -25.69361353241580304 ) ) ;
#849 = DIRECTION ( 'NONE',  ( 1.000000000000000000, 0.000000000000000000, -0.000000000000000000 ) ) ;
#850 = DIRECTION ( 'NONE',  ( 0.000000000000000000, 0.000000000000000000, 1.000000000000000000 ) ) ;
#851 = CARTESIAN_POINT ( 'NONE',  ( 87.74278500247204704, 111.0010834413667453, 71.13281249985656984 ) ) ;
#852 = DIRECTION ( 'NONE',  ( 0.000000000000000000, 0.000000000000000000, -1.000000000000000000 ) ) ;
#853 = CARTESIAN_POINT ( 'NONE',  ( 113.4920585194047078, 104.4775165427241461, -100.0000000000000142 ) ) ;
#854 = FACE_OUTER_BOUND ( 'NONE', #21177, .T. ) ;
#856 = ORIENTED_EDGE ( 'NONE', *, *, #8614, .F. ) ;
#855 = VERTEX_POINT ( 'NONE', #3153 ) ;
#857 = DIRECTION ( 'NONE',  ( -0.000000000000000000, -0.000000000000000000, -1.000000000000000000 ) ) ;
#858 = VECTOR ( 'NONE', #5187, 1000.000000000000227 ) ;
#859 = DIRECTION ( 'NONE',  ( -1.000000000000000000, 0.000000000000000000, 0.000000000000000000 ) ) ;
#860 = VERTEX_POINT ( 'NONE', #14376 ) ;
#861 = ORIENTED_EDGE ( 'NONE', *, *, #22149, .F. ) ;
#862 = ADVANCED_FACE ( 'NONE', ( #20968 ), #22849, .F. ) ;
#863 = VECTOR ( 'NONE', #10211, 1000.000000000000000 ) ;
#864 = FACE_BOUND ( 'NONE', #3431, .T. ) ;
#865 = CARTESIAN_POINT ( 'NONE',  ( -260.0000000000001137, -220.0000000000000853, 90.00000000000001421 ) ) ;
#866 = EDGE_CURVE ( 'NONE', #16598, #10685, #5021, .T. ) ;
#867 = VECTOR ( 'NONE', #14346, 1000.000000000000227 ) ;
#868 = ORIENTED_EDGE ( 'NONE', *, *, #1961, .F. ) ;
#869 = ORIENTED_EDGE ( 'NONE', *, *, #14849, .F. ) ;
#870 = DIRECTION ( 'NONE',  ( 0.000000000000000000, 0.000000000000000000, -1.000000000000000000 ) ) ;
#871 = DIRECTION ( 'NONE',  ( 1.000000000000000000, 3.469446951953614189E-16, -0.000000000000000000 ) ) ;
#872 = DIRECTION ( 'NONE',  ( -0.8916010070299673629, 0.4528218681370723142, 0.000000000000000000 ) ) ;
#873 = DIRECTION ( 'NONE',  ( 0.9711705445023437466, -0.2383857661250380899, 0.000000000000000000 ) ) ;
#874 = VECTOR ( 'NONE', #17839, 1000.000000000000000 ) ;
#875 = DIRECTION ( 'NONE',  ( -1.000000000000000000, 0.000000000000000000, 0.000000000000000000 ) ) ;
#876 = PLANE ( 'NONE',  #27398 ) ;
#877 = CARTESIAN_POINT ( 'NONE',  ( -199.5809478526699650, 61.42778479158862126, -28.44561038857050761 ) ) ;
#878 = AXIS2_PLACEMENT_3D ( 'NONE', #9764, #20527, #852 ) ;
#879 = FACE_OUTER_BOUND ( 'NONE', #7048, .T. ) ;
#880 = FACE_OUTER_BOUND ( 'NONE', #24338, .T. ) ;
#881 = DIRECTION ( 'NONE',  ( -1.000000000000000000, 0.000000000000000000, 0.000000000000000000 ) ) ;
#882 = FACE_OUTER_BOUND ( 'NONE', #28083, .T. ) ;
#883 = VERTEX_POINT ( 'NONE', #24724 ) ;
#884 = CARTESIAN_POINT ( 'NONE',  ( -26.22291647523108438, 23.54903675176048594, -45.00000000000000000 ) ) ;
#885 = EDGE_CURVE ( 'NONE', #13594, #27610, #20406, .T. ) ;
#886 = LINE ( 'NONE', #20423, #24026 ) ;
#887 = DIRECTION ( 'NONE',  ( -0.000000000000000000, 1.000000000000000000, -0.000000000000000000 ) ) ;
#888 = EDGE_LOOP ( 'NONE', ( #23960, #2470, #23686, #8733 ) ) ;
#889 = DIRECTION ( 'NONE',  ( 0.000000000000000000, 0.000000000000000000, 1.000000000000000000 ) ) ;
#890 = ORIENTED_EDGE ( 'NONE', *, *, #18434, .F. ) ;
#891 = CARTESIAN_POINT ( 'NONE',  ( -279.3160071107327553, -91.18033988749901653, 0.000000000000000000 ) ) ;
#892 = AXIS2_PLACEMENT_3D ( 'NONE', #17470, #382, #19632 ) ;
#893 = CARTESIAN_POINT ( 'NONE',  ( 349.0018770490533484, 96.44595867864246941, -145.0000000000000000 ) ) ;
#894 = EDGE_CURVE ( 'NONE', #10441, #6349, #7345, .T. ) ;
#895 = EDGE_LOOP ( 'NONE', ( #24720, #21350 ) ) ;
#896 = AXIS2_PLACEMENT_3D ( 'NONE', #9883, #3402, #7727 ) ;
#897 = ORIENTED_EDGE ( 'NONE', *, *, #21725, .F. ) ;
#898 = CARTESIAN_POINT ( 'NONE',  ( 157.9999999999998010, 236.0472500450420341, 45.00000000000000000 ) ) ;
#899 = VECTOR ( 'NONE', #15523, 1000.000000000000000 ) ;
#900 = EDGE_CURVE ( 'NONE', #19228, #8289, #8468, .T. ) ;
#901 = DIRECTION ( 'NONE',  ( 0.000000000000000000, -1.000000000000000000, 0.000000000000000000 ) ) ;
#902 = PLANE ( 'NONE',  #17386 ) ;
#903 = ORIENTED_EDGE ( 'NONE', *, *, #6405, .T. ) ;
#904 = LINE ( 'NONE', #22604, #27037 ) ;
#905 = VERTEX_POINT ( 'NONE', #16805 ) ;
#906 = CARTESIAN_POINT ( 'NONE',  ( 157.4999999999998579, 125.9546872184859012, -45.00000000000000000 ) ) ;
#907 = CIRCLE ( 'NONE', #10544, 30.00000000000000000 ) ;
#908 = FACE_OUTER_BOUND ( 'NONE', #24115, .T. ) ;
#909 = DIRECTION ( 'NONE',  ( 0.000000000000000000, 0.000000000000000000, 1.000000000000000000 ) ) ;
#910 = CARTESIAN_POINT ( 'NONE',  ( 7.502017008525952768, 138.6551571308461348, -15.00000000000000000 ) ) ;
#911 = LINE ( 'NONE', #2923, #8654 ) ;
#912 = EDGE_CURVE ( 'NONE', #25311, #7612, #22460, .T. ) ;
#913 = DIRECTION ( 'NONE',  ( 0.7071067811867438602, 8.659560562352529298E-17, 0.7071067811863512853 ) ) ;
#914 = CARTESIAN_POINT ( 'NONE',  ( 162.2068797070720905, 207.3581635649740917, -139.6159404653925549 ) ) ;
#915 = EDGE_LOOP ( 'NONE', ( #27754, #21554, #14846, #21946, #26433, #23940, #8844, #5653, #4028, #10467, #1807, #20190 ) ) ;
#916 = VECTOR ( 'NONE', #2379, 1000.000000000000114 ) ;
#917 = FACE_OUTER_BOUND ( 'NONE', #15898, .T. ) ;
#918 = DIRECTION ( 'NONE',  ( 0.000000000000000000, -1.000000000000000000, 0.000000000000000000 ) ) ;
#919 = LINE ( 'NONE', #10110, #24476 ) ;
#920 = ORIENTED_EDGE ( 'NONE', *, *, #8489, .F. ) ;
#921 = DIRECTION ( 'NONE',  ( 4.540956701092242152E-16, 1.000000000000000000, 0.000000000000000000 ) ) ;
#922 = CIRCLE ( 'NONE', #10088, 68.83858790703926900 ) ;
#923 = ORIENTED_EDGE ( 'NONE', *, *, #23688, .T. ) ;
#924 = EDGE_CURVE ( 'NONE', #19307, #27610, #27839, .T. ) ;
#925 = AXIS2_PLACEMENT_3D ( 'NONE', #9640, #25275, #15970 ) ;
#926 = DIRECTION ( 'NONE',  ( -0.8916010070293409751, -0.4528218681383056610, 0.000000000000000000 ) ) ;
#927 = CARTESIAN_POINT ( 'NONE',  ( 158.0000000000008527, 123.7007497147323960, 45.00000000000000000 ) ) ;
#928 = ORIENTED_EDGE ( 'NONE', *, *, #17521, .F. ) ;
#929 = DIRECTION ( 'NONE',  ( 1.000000000000000000, 0.000000000000000000, 0.000000000000000000 ) ) ;
#930 = ORIENTED_EDGE ( 'NONE', *, *, #5858, .F. ) ;
#931 = CARTESIAN_POINT ( 'NONE',  ( 158.0000000000012221, 88.59049960963380954, 45.00000000000000000 ) ) ;
#932 = CARTESIAN_POINT ( 'NONE',  ( -266.6125751775834942, -170.7865253013266056, -104.7181492081291765 ) ) ;
#933 = EDGE_LOOP ( 'NONE', ( #25332, #26932, #17589, #8882, #1061, #19824, #4317, #18042 ) ) ;
#934 = ORIENTED_EDGE ( 'NONE', *, *, #23204, .T. ) ;
#935 = CARTESIAN_POINT ( 'NONE',  ( 157.4999999999998579, 171.0964373536126573, -45.00000000000000000 ) ) ;
#936 = ORIENTED_EDGE ( 'NONE', *, *, #5812, .F. ) ;
#937 = ADVANCED_FACE ( 'NONE', ( #14514, #19097, #8178, #25421, #14651 ), #23838, .F. ) ;
#938 = CIRCLE ( 'NONE', #21121, 18.91107291867258411 ) ;
#939 = ADVANCED_FACE ( 'NONE', ( #16943 ), #28267, .F. ) ;
#940 = ORIENTED_EDGE ( 'NONE', *, *, #27692, .F. ) ;
#941 = ORIENTED_EDGE ( 'NONE', *, *, #23394, .T. ) ;
#942 = CARTESIAN_POINT ( 'NONE',  ( 158.0000000000014495, 66.01962454207041731, 45.00000000000000000 ) ) ;
#943 = VECTOR ( 'NONE', #21161, 1000.000000000000000 ) ;
#944 = DIRECTION ( 'NONE',  ( -0.000000000000000000, -1.000000000000000000, -0.000000000000000000 ) ) ;
#945 = DIRECTION ( 'NONE',  ( 1.000000000000000000, 0.000000000000000000, 0.000000000000000000 ) ) ;
#946 = EDGE_CURVE ( 'NONE', #12013, #2614, #5471, .T. ) ;
#947 = CARTESIAN_POINT ( 'NONE',  ( 104.1118574119011555, 122.0584436052145918, -84.84374999967577935 ) ) ;
#948 = CARTESIAN_POINT ( 'NONE',  ( 187.4999999999996305, 526.4263741777961059, -74.99999999999995737 ) ) ;
#949 = DIRECTION ( 'NONE',  ( 0.000000000000000000, -1.000000000000000000, 0.000000000000000000 ) ) ;
#950 = FACE_OUTER_BOUND ( 'NONE', #5628, .T. ) ;
#951 = FACE_OUTER_BOUND ( 'NONE', #17284, .T. ) ;
#952 = CARTESIAN_POINT ( 'NONE',  ( -175.0000000000000000, -120.0000000000001847, -64.00000000000000000 ) ) ;
#953 = LINE ( 'NONE', #18483, #6794 ) ;
#954 = LINE ( 'NONE', #12451, #19901 ) ;
#955 = ORIENTED_EDGE ( 'NONE', *, *, #8077, .T. ) ;
#956 = EDGE_CURVE ( 'NONE', #7560, #13193, #23407, .T. ) ;
#957 = AXIS2_PLACEMENT_3D ( 'NONE', #27536, #849, #25400 ) ;
#958 = DIRECTION ( 'NONE',  ( 0.4528218681379303501, -0.8916010070295316003, 0.000000000000000000 ) ) ;
#959 = DIRECTION ( 'NONE',  ( 0.000000000000000000, -1.000000000000000000, 0.000000000000000000 ) ) ;
#960 = ADVANCED_FACE ( 'NONE', ( #5736 ), #3715, .T. ) ;
#961 = FACE_OUTER_BOUND ( 'NONE', #3277, .T. ) ;
#962 = VERTEX_POINT ( 'NONE', #1425 ) ;
#963 = VECTOR ( 'NONE', #22515, 1000.000000000000000 ) ;
#964 = DIRECTION ( 'NONE',  ( 0.000000000000000000, 1.000000000000000000, -0.000000000000000000 ) ) ;
#965 = ORIENTED_EDGE ( 'NONE', *, *, #5174, .F. ) ;
#966 = DIRECTION ( 'NONE',  ( -0.000000000000000000, -0.000000000000000000, -1.000000000000000000 ) ) ;
#967 = ORIENTED_EDGE ( 'NONE', *, *, #14592, .T. ) ;
#968 = VERTEX_POINT ( 'NONE', #19378 ) ;
#969 = VERTEX_POINT ( 'NONE', #17222 ) ;
#970 = VERTEX_POINT ( 'NONE', #8325 ) ;
#971 = CARTESIAN_POINT ( 'NONE',  ( -81.43952348080793513, 136.3896988708861215, 13.49547953233103392 ) ) ;
#972 = CARTESIAN_POINT ( 'NONE',  ( 157.9999999999996589, 278.6811251726610976, 45.00000000000000000 ) ) ;
#973 = CARTESIAN_POINT ( 'NONE',  ( -211.6502095576267948, -220.0000000000000568, -92.65159606798890479 ) ) ;
#974 = TOROIDAL_SURFACE ( 'NONE', #19304, 44.99999999999999289, 5.000000000000000000 ) ;
#975 = FACE_OUTER_BOUND ( 'NONE', #15503, .T. ) ;
#976 = DIRECTION ( 'NONE',  ( -0.000000000000000000, 0.000000000000000000, -1.000000000000000000 ) ) ;
#977 = AXIS2_PLACEMENT_3D ( 'NONE', #1019, #14248, #3304 ) ;
#978 = CARTESIAN_POINT ( 'NONE',  ( -295.0000000000001137, -170.0000000000001137, 60.00000000000002842 ) ) ;
#979 = CARTESIAN_POINT ( 'NONE',  ( 65.00000000000000000, -170.0000000000000568, 64.00000000000004263 ) ) ;
#980 = CARTESIAN_POINT ( 'NONE',  ( -122.9477694338266360, 132.7606495686108872, -14.33686514723054373 ) ) ;
#981 = CARTESIAN_POINT ( 'NONE',  ( 158.0000000000016769, 47.95662448201407102, 45.00000000000000000 ) ) ;
#982 = DIRECTION ( 'NONE',  ( -0.000000000000000000, 0.000000000000000000, -1.000000000000000000 ) ) ;
#983 = EDGE_CURVE ( 'NONE', #14755, #9116, #3862, .T. ) ;
#984 = CARTESIAN_POINT ( 'NONE',  ( -260.0000000000001137, -157.0000000000000284, 60.00000000000002132 ) ) ;
#985 = DIRECTION ( 'NONE',  ( -1.000000000000000000, 4.540956701092242152E-16, 0.000000000000000000 ) ) ;
#986 = CARTESIAN_POINT ( 'NONE',  ( 33.10302365956999182, 203.2034914284457159, -15.00000000000000000 ) ) ;
#987 = ADVANCED_FACE ( 'NONE', ( #25840 ), #26568, .T. ) ;
#988 = DIRECTION ( 'NONE',  ( 0.000000000000000000, 0.5150380749100563760, 0.8571673007021110013 ) ) ;
#989 = CARTESIAN_POINT ( 'NONE',  ( 119.9999999999999147, 140.0000000000000000, -100.0000000000000142 ) ) ;
#990 = DIRECTION ( 'NONE',  ( 0.000000000000000000, 0.000000000000000000, 1.000000000000000000 ) ) ;
#992 = ORIENTED_EDGE ( 'NONE', *, *, #15561, .F. ) ;
#991 = VERTEX_POINT ( 'NONE', #4002 ) ;
#993 = CIRCLE ( 'NONE', #27137, 166.0121251338587172 ) ;
#994 = CARTESIAN_POINT ( 'NONE',  ( -55.40193461144291831, 169.7519813918499665, 45.00000000000000000 ) ) ;
#995 = EDGE_LOOP ( 'NONE', ( #6255, #19786, #27111, #10655, #13692 ) ) ;
#996 = VECTOR ( 'NONE', #5623, 1000.000000000000000 ) ;
#997 = EDGE_LOOP ( 'NONE', ( #19109, #27348, #25490, #11756, #45, #10235 ) ) ;
#998 = CIRCLE ( 'NONE', #19800, 5.000000000000004441 ) ;
#999 = VERTEX_POINT ( 'NONE', #1707 ) ;
#1000 = ORIENTED_EDGE ( 'NONE', *, *, #28394, .T. ) ;
#1001 = DIRECTION ( 'NONE',  ( -1.850371707708594316E-16, 1.000000000000000000, 0.000000000000000000 ) ) ;
#1002 = DIRECTION ( 'NONE',  ( -0.000000000000000000, -0.000000000000000000, -1.000000000000000000 ) ) ;
#1003 = EDGE_CURVE ( 'NONE', #18388, #2119, #10337, .T. ) ;
#1004 = DIRECTION ( 'NONE',  ( -0.7892793597178160425, -0.6140342761796236948, 0.000000000000000000 ) ) ;
#1005 = CARTESIAN_POINT ( 'NONE',  ( 157.9999999999999716, 210.9684999699701393, 45.00000000000000000 ) ) ;
#1006 = CARTESIAN_POINT ( 'NONE',  ( -20.22388308534250712, 128.4000958562204460, -17.33254599016412101 ) ) ;
#1007 = AXIS2_PLACEMENT_3D ( 'NONE', #4086, #12870, #21613 ) ;
#1008 = DIRECTION ( 'NONE',  ( -0.5555587585212683477, -0.8314772792026894344, -0.000000000000000000 ) ) ;
#1009 = EDGE_CURVE ( 'NONE', #27752, #3252, #23271, .T. ) ;
#1010 = AXIS2_PLACEMENT_3D ( 'NONE', #4400, #24228, #2669 ) ;
#1011 = DIRECTION ( 'NONE',  ( 0.000000000000000000, 0.000000000000000000, 1.000000000000000000 ) ) ;
#1012 = AXIS2_PLACEMENT_3D ( 'NONE', #20983, #14669, #5618 ) ;
#1013 = CARTESIAN_POINT ( 'NONE',  ( 157.9999999999997442, 254.1102501050980322, 45.00000000000000000 ) ) ;
#1014 = EDGE_CURVE ( 'NONE', #9382, #18102, #26729, .T. ) ;
#1015 = AXIS2_PLACEMENT_3D ( 'NONE', #23644, #1520, #25373 ) ;
#1016 = ADVANCED_FACE ( 'NONE', ( #21677 ), #10767, .F. ) ;
#1017 = CARTESIAN_POINT ( 'NONE',  ( 110.0398043607047640, 203.3530833388224153, -139.3076717160242595 ) ) ;
#1018 = EDGE_CURVE ( 'NONE', #9020, #6014, #12368, .T. ) ;
#1019 = CARTESIAN_POINT ( 'NONE',  ( 139.9999999999999716, -120.0000000000000284, 70.00000000000001421 ) ) ;
#1020 = FACE_OUTER_BOUND ( 'NONE', #12119, .T. ) ;
#1021 = LINE ( 'NONE', #26890, #24051 ) ;
#1022 = ORIENTED_EDGE ( 'NONE', *, *, #15495, .T. ) ;
#1023 = CARTESIAN_POINT ( 'NONE',  ( 157.9999999999998010, 238.5551250525490161, 45.00000000000000000 ) ) ;
#1024 = CARTESIAN_POINT ( 'NONE',  ( -242.2202452113856737, 73.32912780459425051, 5.047888127315641960 ) ) ;
#1025 = CARTESIAN_POINT ( 'NONE',  ( 158.0000000000009948, 108.6534996696901345, 45.00000000000000000 ) ) ;
#1026 = ORIENTED_EDGE ( 'NONE', *, *, #13555, .T. ) ;
#1027 = DIRECTION ( 'NONE',  ( -1.387778780781445429E-16, 1.387778780781445429E-16, 1.000000000000000000 ) ) ;
#1028 = ORIENTED_EDGE ( 'NONE', *, *, #14203, .T. ) ;
#1029 = VECTOR ( 'NONE', #18745, 1000.000000000000114 ) ;
#1030 = AXIS2_PLACEMENT_3D ( 'NONE', #19427, #23883, #12979 ) ;
#1031 = CARTESIAN_POINT ( 'NONE',  ( 84.91648909967247505, 110.3843228249417479, 70.37109374985131183 ) ) ;
#1032 = DIRECTION ( 'NONE',  ( -1.000000000000000000, 0.000000000000000000, -0.000000000000000000 ) ) ;
#1033 = EDGE_LOOP ( 'NONE', ( #26255, #14234, #2632, #13709 ) ) ;
#1034 = AXIS2_PLACEMENT_3D ( 'NONE', #27642, #24944, #3377 ) ;
#1035 = ORIENTED_EDGE ( 'NONE', *, *, #2765, .F. ) ;
#1036 = FACE_OUTER_BOUND ( 'NONE', #18183, .T. ) ;
#1037 = TOROIDAL_SURFACE ( 'NONE', #14808, 18.46313063346208239, 2.000000000000000000 ) ;
#1038 = DIRECTION ( 'NONE',  ( 0.000000000000000000, 0.000000000000000000, 1.000000000000000000 ) ) ;
#1039 = LINE ( 'NONE', #9809, #10502 ) ;
#1040 = ORIENTED_EDGE ( 'NONE', *, *, #11015, .F. ) ;
#1041 = CYLINDRICAL_SURFACE ( 'NONE', #20624, 30.00000000000002842 ) ;
#1042 = ORIENTED_EDGE ( 'NONE', *, *, #1210, .T. ) ;
#1043 = DIRECTION ( 'NONE',  ( 0.8916010070293584056, -0.4528218681382712996, 0.000000000000000000 ) ) ;
#1044 = ADVANCED_FACE ( 'NONE', ( #22244 ), #4850, .F. ) ;
#1045 = ADVANCED_FACE ( 'NONE', ( #24257 ), #7016, .F. ) ;
#1046 = ADVANCED_FACE ( 'NONE', ( #26122 ), #416, .T. ) ;
#1047 = DIRECTION ( 'NONE',  ( 0.8916010070298258094, 0.4528218681373508137, 0.000000000000000000 ) ) ;
#1048 = CARTESIAN_POINT ( 'NONE',  ( 116.5224093497741364, 227.6536686473013447, 45.00000000000000000 ) ) ;
#1049 = CARTESIAN_POINT ( 'NONE',  ( 157.9999999999998295, 226.0157500150140208, -45.00000000000000000 ) ) ;
#1050 = FACE_OUTER_BOUND ( 'NONE', #10538, .T. ) ;
#1051 = VECTOR ( 'NONE', #4355, 999.9999999999998863 ) ;
#1052 = FACE_OUTER_BOUND ( 'NONE', #20368, .T. ) ;
#1053 = DIRECTION ( 'NONE',  ( 0.000000000000000000, -1.000000000000000000, 0.000000000000000000 ) ) ;
#1054 = ORIENTED_EDGE ( 'NONE', *, *, #15982, .F. ) ;
#1055 = CIRCLE ( 'NONE', #14355, 15.26911010665567225 ) ;
#1056 = CARTESIAN_POINT ( 'NONE',  ( 157.4999999999996874, 271.4114376538935289, 45.00000000000000000 ) ) ;
#1057 = ADVANCED_FACE ( 'NONE', ( #26541 ), #2408, .F. ) ;
#1058 = CARTESIAN_POINT ( 'NONE',  ( -225.3736415174280978, 135.7651958811247539, 14.97905406095859426 ) ) ;
#1059 = AXIS2_PLACEMENT_3D ( 'NONE', #4720, #7463, #22546 ) ;
#1060 = DIRECTION ( 'NONE',  ( -0.8916010070297446521, -0.4528218681375106858, 0.000000000000000000 ) ) ;
#1061 = ORIENTED_EDGE ( 'NONE', *, *, #4761, .T. ) ;
#1062 = LINE ( 'NONE', #26784, #6383 ) ;
#1063 = VERTEX_POINT ( 'NONE', #2268 ) ;
#1064 = EDGE_CURVE ( 'NONE', #27217, #21245, #19801, .T. ) ;
#1065 = CARTESIAN_POINT ( 'NONE',  ( -110.3221550338875687, 20.24192588826927164, 93.88690167569080813 ) ) ;
#1066 = PLANE ( 'NONE',  #8262 ) ;
#1067 = LINE ( 'NONE', #21162, #5729 ) ;
#1068 = ORIENTED_EDGE ( 'NONE', *, *, #27119, .F. ) ;
#1069 = LINE ( 'NONE', #18869, #7867 ) ;
#1070 = VERTEX_POINT ( 'NONE', #26265 ) ;
#1071 = CARTESIAN_POINT ( 'NONE',  ( -107.6172385141402259, 133.6752736189426969, 15.67102466709354935 ) ) ;
#1072 = DIRECTION ( 'NONE',  ( -0.000000000000000000, -0.000000000000000000, -1.000000000000000000 ) ) ;
#1073 = EDGE_LOOP ( 'NONE', ( #5385, #17781, #693, #27335 ) ) ;
#1074 = VECTOR ( 'NONE', #4601, 1000.000000000000000 ) ;
#1075 = ORIENTED_EDGE ( 'NONE', *, *, #26791, .T. ) ;
#1076 = FACE_OUTER_BOUND ( 'NONE', #21023, .T. ) ;
#1077 = EDGE_LOOP ( 'NONE', ( #8320, #5448, #967, #19763 ) ) ;
#1078 = AXIS2_PLACEMENT_3D ( 'NONE', #16858, #26030, #8234 ) ;
#1079 = EDGE_LOOP ( 'NONE', ( #25472, #803, #15589, #7233 ) ) ;
#1080 = ORIENTED_EDGE ( 'NONE', *, *, #17394, .F. ) ;
#1081 = AXIS2_PLACEMENT_3D ( 'NONE', #9761, #10179, #23111 ) ;
#1082 = CARTESIAN_POINT ( 'NONE',  ( 109.1380356258735134, 251.5976846382455676, 37.70750237629315649 ) ) ;
#1083 = ADVANCED_FACE ( 'NONE', ( #13352 ), #125, .F. ) ;
#1084 = CARTESIAN_POINT ( 'NONE',  ( 111.9999999999999289, 218.9999999999996874, 45.00000000000000000 ) ) ;
#1085 = CARTESIAN_POINT ( 'NONE',  ( 9.999999999999738876, -50.00000000000004263, 98.28427124746191623 ) ) ;
#1086 = DIRECTION ( 'NONE',  ( 0.4528218681371510290, -0.8916010070299273949, 0.000000000000000000 ) ) ;
#1087 = CARTESIAN_POINT ( 'NONE',  ( -180.0000000000000000, -40.00000000000004974, -100.0000000000000142 ) ) ;
#1088 = DIRECTION ( 'NONE',  ( -0.000000000000000000, -0.000000000000000000, -1.000000000000000000 ) ) ;
#1089 = LINE ( 'NONE', #13758, #13150 ) ;
#1090 = DIRECTION ( 'NONE',  ( -0.9784193629480828491, -0.2066290158914464437, 0.000000000000000000 ) ) ;
#1091 = LINE ( 'NONE', #12310, #4041 ) ;
#1092 = CARTESIAN_POINT ( 'NONE',  ( -56.65306767071049165, 63.08575069354419185, -45.00000000000000000 ) ) ;
#1093 = ORIENTED_EDGE ( 'NONE', *, *, #14518, .F. ) ;
#1094 = VECTOR ( 'NONE', #24258, 1000.000000000000000 ) ;
#1095 = EDGE_CURVE ( 'NONE', #18723, #12774, #4427, .T. ) ;
#1096 = EDGE_CURVE ( 'NONE', #27590, #27147, #25666, .T. ) ;
#1097 = CARTESIAN_POINT ( 'NONE',  ( 90.99996269066551235, 240.0000000000000853, -6.657450422703546700 ) ) ;
#1098 = DIRECTION ( 'NONE',  ( 1.000000000000000000, 0.000000000000000000, 0.000000000000000000 ) ) ;
#1099 =( NAMED_UNIT ( * ) PLANE_ANGLE_UNIT ( ) SI_UNIT ( $, .RADIAN. ) );
#1100 = CARTESIAN_POINT ( 'NONE',  ( -76.25760768171836901, 154.8982798170083299, -15.00000000000000000 ) ) ;
#1101 = VECTOR ( 'NONE', #18023, 1000.000000000000000 ) ;
#1102 = ORIENTED_EDGE ( 'NONE', *, *, #26834, .F. ) ;
#1103 = FACE_OUTER_BOUND ( 'NONE', #1724, .T. ) ;
#1104 = ORIENTED_EDGE ( 'NONE', *, *, #11937, .F. ) ;
#1105 = DIRECTION ( 'NONE',  ( 0.000000000000000000, 0.000000000000000000, -1.000000000000000000 ) ) ;
#1106 = EDGE_LOOP ( 'NONE', ( #25794, #23031, #16354, #299 ) ) ;
#1107 = ADVANCED_FACE ( 'NONE', ( #10905 ), #6589, .F. ) ;
#1108 = ORIENTED_EDGE ( 'NONE', *, *, #8766, .T. ) ;
#1109 = ADVANCED_FACE ( 'NONE', ( #4709 ), #13494, .F. ) ;
#1110 = ORIENTED_EDGE ( 'NONE', *, *, #10106, .T. ) ;
#1111 = VERTEX_POINT ( 'NONE', #20083 ) ;
#1112 = ORIENTED_EDGE ( 'NONE', *, *, #27771, .F. ) ;
#1113 = CARTESIAN_POINT ( 'NONE',  ( -137.6741556889342633, 128.9596988076234823, 15.73777296567075901 ) ) ;
#1114 = VECTOR ( 'NONE', #25456, 1000.000000000000000 ) ;
#1115 = CARTESIAN_POINT ( 'NONE',  ( -15.28840184913744515, 9.956927649352207865, -45.00000000000000000 ) ) ;
#1116 = LINE ( 'NONE', #16360, #2392 ) ;
#1117 = CARTESIAN_POINT ( 'NONE',  ( -47.64428992525972717, 132.2658675021500301, -15.94853873366968955 ) ) ;
#1118 = VECTOR ( 'NONE', #26590, 1000.000000000000114 ) ;
#1119 = CARTESIAN_POINT ( 'NONE',  ( 157.4999999999997442, 251.3484375938375024, 45.00000000000000000 ) ) ;
#1120 = DIRECTION ( 'NONE',  ( -0.000000000000000000, -1.000000000000000000, -0.000000000000000000 ) ) ;
#1121 = DIRECTION ( 'NONE',  ( 0.8379557447115634217, 0.5457381880580551847, -0.000000000000000000 ) ) ;
#1122 = DIRECTION ( 'NONE',  ( -1.000000000000000000, 0.000000000000000000, -9.251858538542972814E-17 ) ) ;
#1123 = DIRECTION ( 'NONE',  ( -0.000000000000000000, -0.000000000000000000, 1.000000000000000000 ) ) ;
#1124 = FACE_OUTER_BOUND ( 'NONE', #12500, .T. ) ;
#1125 = SURFACE_STYLE_USAGE ( .BOTH. , #5432 ) ;
#1126 = DIRECTION ( 'NONE',  ( -0.9659258262890652036, 0.2588190451025321748, 0.000000000000000000 ) ) ;
#1127 = EDGE_LOOP ( 'NONE', ( #28264, #5730, #17065, #9026 ) ) ;
#1128 = EDGE_CURVE ( 'NONE', #12217, #24673, #907, .T. ) ;
#1129 = LINE ( 'NONE', #5860, #6839 ) ;
#1130 = CARTESIAN_POINT ( 'NONE',  ( -186.0376809321689393, 105.9168515575387062, 32.47349478036296233 ) ) ;
#1131 = DIRECTION ( 'NONE',  ( 0.000000000000000000, 0.000000000000000000, -1.000000000000000000 ) ) ;
#1133 = ORIENTED_EDGE ( 'NONE', *, *, #12866, .F. ) ;
#1132 = VERTEX_POINT ( 'NONE', #26686 ) ;
#1134 = VECTOR ( 'NONE', #17507, 1000.000000000000000 ) ;
#1135 = LINE ( 'NONE', #994, #11133 ) ;
#1136 = ORIENTED_EDGE ( 'NONE', *, *, #1662, .T. ) ;
#1137 = ORIENTED_EDGE ( 'NONE', *, *, #10876, .F. ) ;
#1138 = AXIS2_PLACEMENT_3D ( 'NONE', #15635, #24526, #24378 ) ;
#1139 = VERTEX_POINT ( 'NONE', #23978 ) ;
#1140 = ORIENTED_EDGE ( 'NONE', *, *, #15633, .F. ) ;
#1141 = ORIENTED_EDGE ( 'NONE', *, *, #26039, .F. ) ;
#1142 = DIRECTION ( 'NONE',  ( -0.000000000000000000, -0.000000000000000000, -1.000000000000000000 ) ) ;
#1143 = ADVANCED_FACE ( 'NONE', ( #13642, #22387 ), #8608, .F. ) ;
#1144 = DIRECTION ( 'NONE',  ( -0.000000000000000000, 0.000000000000000000, -1.000000000000000000 ) ) ;
#1145 = EDGE_CURVE ( 'NONE', #3426, #23655, #17362, .T. ) ;
#1146 = B_SPLINE_CURVE_WITH_KNOTS ( 'NONE', 3,
 ( #2986, #11778, #20518, #7017, #841, #18510, #9609, #18369, #24975, #11341, #5288, #27256, #7596, #417, #17936, #16878, #3261, #27389, #1643, #3936, #14876, #10412 ),
 .UNSPECIFIED., .F., .F.,
 ( 4, 2, 2, 2, 2, 2, 2, 2, 2, 2, 4 ),
 ( 0.000000000000000000, 0.006705097167734689993, 0.01341019433546937999, 0.01676274291933672195, 0.02011529150320406911, 0.02682038867093874610, 0.03352548583867343002, 0.03687803442254078412, 0.04023058300640813129, 0.04693568017414279786, 0.05364077734187745750 ),
 .UNSPECIFIED. ) ;
#1147 = DIRECTION ( 'NONE',  ( -0.000000000000000000, -1.000000000000000000, -0.000000000000000000 ) ) ;
#1148 = VECTOR ( 'NONE', #9574, 1000.000000000000000 ) ;
#1149 = EDGE_CURVE ( 'NONE', #12999, #26726, #19664, .T. ) ;
#1150 = VECTOR ( 'NONE', #20971, 1000.000000000000000 ) ;
#1151 = LINE ( 'NONE', #27287, #12102 ) ;
#1152 = LINE ( 'NONE', #23410, #5980 ) ;
#1153 = CARTESIAN_POINT ( 'NONE',  ( -21.33210486176665910, 0.000000000000000000, 99.00000000000000000 ) ) ;
#1154 = CIRCLE ( 'NONE', #8503, 7.499999999999992895 ) ;
#1155 = DIRECTION ( 'NONE',  ( -0.8916010070298455714, 0.4528218681373120669, 0.000000000000000000 ) ) ;
#1156 = CARTESIAN_POINT ( 'NONE',  ( -219.5652642369064722, 71.26897287455133778, -22.07429503402158488 ) ) ;
#1157 = CARTESIAN_POINT ( 'NONE',  ( 112.5442897163041636, 200.1067580395811092, -145.3931298709317446 ) ) ;
#1158 = CARTESIAN_POINT ( 'NONE',  ( 158.0000000000013642, 76.05112457209858690, -45.00000000000000000 ) ) ;
#1159 = DIRECTION ( 'NONE',  ( 0.000000000000000000, 0.000000000000000000, -1.000000000000000000 ) ) ;
#1160 = FACE_OUTER_BOUND ( 'NONE', #21524, .T. ) ;
#1161 = ORIENTED_EDGE ( 'NONE', *, *, #20118, .T. ) ;
#1162 = CARTESIAN_POINT ( 'NONE',  ( 116.8936292565958439, 233.3691281929210959, -99.51164200157825235 ) ) ;
#1163 = DIRECTION ( 'NONE',  ( 0.05364526231778980747, 0.9985600561963489108, -0.000000000000000000 ) ) ;
#1164 = EDGE_LOOP ( 'NONE', ( #14157, #27836 ) ) ;
#1165 = DIRECTION ( 'NONE',  ( 0.000000000000000000, 0.000000000000000000, 1.000000000000000000 ) ) ;
#1166 = VECTOR ( 'NONE', #3193, 1000.000000000000000 ) ;
#1167 = ORIENTED_EDGE ( 'NONE', *, *, #1977, .F. ) ;
#1168 = AXIS2_PLACEMENT_3D ( 'NONE', #14174, #20345, #22928 ) ;
#1169 = VECTOR ( 'NONE', #12343, 1000.000000000000114 ) ;
#1170 = ORIENTED_EDGE ( 'NONE', *, *, #1303, .T. ) ;
#1171 = CARTESIAN_POINT ( 'NONE',  ( 432.4999999999996589, 19.41075299063184900, 95.49671038392668265 ) ) ;
#1172 = CARTESIAN_POINT ( 'NONE',  ( 40.99999999999999289, 0.000000000000000000, 0.000000000000000000 ) ) ;
#1173 = ORIENTED_EDGE ( 'NONE', *, *, #21099, .F. ) ;
#1174 = EDGE_CURVE ( 'NONE', #22407, #11012, #9175, .T. ) ;
#1175 = VECTOR ( 'NONE', #2149, 1000.000000000000000 ) ;
#1176 = VERTEX_POINT ( 'NONE', #7595 ) ;
#1177 = DIRECTION ( 'NONE',  ( 1.000000000000000000, 0.000000000000000000, -0.000000000000000000 ) ) ;
#1178 = ADVANCED_FACE ( 'NONE', ( #975 ), #7163, .F. ) ;
#1179 = LINE ( 'NONE', #2764, #6588 ) ;
#1180 = EDGE_CURVE ( 'NONE', #20032, #27491, #12053, .T. ) ;
#1181 = CARTESIAN_POINT ( 'NONE',  ( -210.0000000000000568, -210.8114316696540982, -89.99999999999987210 ) ) ;
#1182 = EDGE_LOOP ( 'NONE', ( #21901, #2724, #8353, #8644 ) ) ;
#1183 = DIRECTION ( 'NONE',  ( 0.9506505318133497973, -0.3102637045530707294, 0.000000000000000000 ) ) ;
#1184 = ORIENTED_EDGE ( 'NONE', *, *, #2530, .F. ) ;
#1185 = CARTESIAN_POINT ( 'NONE',  ( -37.82257053376181233, 36.92584315232891612, 99.00000000000000000 ) ) ;
#1186 = FACE_OUTER_BOUND ( 'NONE', #26674, .T. ) ;
#1187 = AXIS2_PLACEMENT_3D ( 'NONE', #15807, #5001, #8754 ) ;
#1188 = PLANE ( 'NONE',  #15906 ) ;
#1189 = FACE_OUTER_BOUND ( 'NONE', #15125, .T. ) ;
#1190 = AXIS2_PLACEMENT_3D ( 'NONE', #25235, #16624, #25381 ) ;
#1191 = CARTESIAN_POINT ( 'NONE',  ( 158.0000000000006537, 143.7637497747887210, 45.00000000000000000 ) ) ;
#1192 = CARTESIAN_POINT ( 'NONE',  ( -185.4366074710545433, 106.2948058035834435, -32.30162111875018383 ) ) ;
#1193 = ORIENTED_EDGE ( 'NONE', *, *, #23218, .T. ) ;
#1194 = FACE_OUTER_BOUND ( 'NONE', #5435, .T. ) ;
#1196 = DIRECTION ( 'NONE',  ( -0.000000000000000000, 1.000000000000000000, -1.387778780781445429E-16 ) ) ;
#1195 = VECTOR ( 'NONE', #9893, 999.9999999999998863 ) ;
#1197 = CARTESIAN_POINT ( 'NONE',  ( -175.0000000000000000, -120.0000000000001705, 70.00000000000001421 ) ) ;
#1198 = DIRECTION ( 'NONE',  ( 0.000000000000000000, -1.000000000000000000, 0.000000000000000000 ) ) ;
#1199 = ORIENTED_EDGE ( 'NONE', *, *, #6700, .F. ) ;
#1200 = CARTESIAN_POINT ( 'NONE',  ( 158.0000000000002558, 181.3818748873943889, 45.00000000000000000 ) ) ;
#1201 = ORIENTED_EDGE ( 'NONE', *, *, #15008, .T. ) ;
#1202 = APPLICATION_CONTEXT ( 'automotive_design' ) ;
#1203 = DIRECTION ( 'NONE',  ( 0.000000000000000000, -1.000000000000000000, 0.000000000000000000 ) ) ;
#1204 = CARTESIAN_POINT ( 'NONE',  ( 157.4999999999994600, 216.2381874887387880, 45.00000000000000000 ) ) ;
#1205 = LINE ( 'NONE', #27617, #12642 ) ;
#1206 = ORIENTED_EDGE ( 'NONE', *, *, #3981, .T. ) ;
#1207 = CARTESIAN_POINT ( 'NONE',  ( 65.00000000000000000, -120.0000000000000711, 70.00000000000001421 ) ) ;
#1208 = CARTESIAN_POINT ( 'NONE',  ( -175.0000000000000000, -150.0000000000000853, -69.99999999999998579 ) ) ;
#1209 = ORIENTED_EDGE ( 'NONE', *, *, #3052, .T. ) ;
#1210 = EDGE_CURVE ( 'NONE', #1637, #378, #24687, .T. ) ;
#1211 = DIRECTION ( 'NONE',  ( 0.000000000000000000, 0.000000000000000000, 1.000000000000000000 ) ) ;
#1212 = CARTESIAN_POINT ( 'NONE',  ( -260.0000000000001137, -157.0000000000000284, 90.00000000000001421 ) ) ;
#1213 = VERTEX_POINT ( 'NONE', #25106 ) ;
#1214 = AXIS2_PLACEMENT_3D ( 'NONE', #8774, #10932, #19691 ) ;
#1215 = VERTEX_POINT ( 'NONE', #5423 ) ;
#1216 = EDGE_CURVE ( 'NONE', #7652, #26924, #15939, .T. ) ;
#1217 = LINE ( 'NONE', #19159, #2597 ) ;
#1218 = ORIENTED_EDGE ( 'NONE', *, *, #16788, .T. ) ;
#1219 = ADVANCED_FACE ( 'NONE', ( #9748 ), #9363, .T. ) ;
#1220 = VERTEX_POINT ( 'NONE', #27527 ) ;
#1221 = AXIS2_PLACEMENT_3D ( 'NONE', #23489, #21469, #12729 ) ;
#1222 = ORIENTED_EDGE ( 'NONE', *, *, #3961, .F. ) ;
#1223 = LINE ( 'NONE', #26946, #1029 ) ;
#1224 = PRODUCT_DEFINITION ( 'UNKNOWN', '', #2378, #1991 ) ;
#1225 = DIRECTION ( 'NONE',  ( 2.312964634635742464E-16, -1.000000000000000000, 2.139922160430262010E-31 ) ) ;
#1226 = FACE_OUTER_BOUND ( 'NONE', #27486, .T. ) ;
#1227 = CARTESIAN_POINT ( 'NONE',  ( 90.92319367352099846, 112.0484670279005570, -72.65625000014701129 ) ) ;
#1228 = LINE ( 'NONE', #27227, #22752 ) ;
#1229 = DIRECTION ( 'NONE',  ( 0.000000000000000000, 0.000000000000000000, -1.000000000000000000 ) ) ;
#1230 = LINE ( 'NONE', #8267, #18652 ) ;
#1231 = LINE ( 'NONE', #27231, #25754 ) ;
#1232 = CARTESIAN_POINT ( 'NONE',  ( 157.4999999999998579, 70.78143705333094715, 45.00000000000000000 ) ) ;
#1233 = DIRECTION ( 'NONE',  ( 1.000000000000000000, 0.000000000000000000, 0.000000000000000000 ) ) ;
#1234 = VECTOR ( 'NONE', #20751, 1000.000000000000000 ) ;
#1235 = VERTEX_POINT ( 'NONE', #5848 ) ;
#1236 = CARTESIAN_POINT ( 'NONE',  ( -20.04511428896995895, 128.4222523959858222, 17.32321537865083982 ) ) ;
#1237 = DIRECTION ( 'NONE',  ( 0.8916010070299476009, 0.4528218681371110610, 0.000000000000000000 ) ) ;
#1238 = CARTESIAN_POINT ( 'NONE',  ( 133.9999999999998295, 242.9999999999997158, 45.00000000000000000 ) ) ;
#1239 = CYLINDRICAL_SURFACE ( 'NONE', #18735, 49.99999999999998579 ) ;
#1240 = CARTESIAN_POINT ( 'NONE',  ( 167.4999999999996589, 494.4107529906318632, -74.99999999999995737 ) ) ;
#1241 = EDGE_CURVE ( 'NONE', #27002, #15645, #1541, .T. ) ;
#1242 = VERTEX_POINT ( 'NONE', #7866 ) ;
#1243 = ADVANCED_FACE ( 'NONE', ( #8010 ), #21077, .F. ) ;
#1244 = CARTESIAN_POINT ( 'NONE',  ( 134.9999999999998579, 220.0000000000000284, -84.99999999999997158 ) ) ;
#1245 = EDGE_LOOP ( 'NONE', ( #25978, #17736, #1694, #18857 ) ) ;
#1246 = CARTESIAN_POINT ( 'NONE',  ( 157.9999999999997726, 241.5708750675630370, 45.00000000000000000 ) ) ;
#1247 = VERTEX_POINT ( 'NONE', #25391 ) ;
#1248 = ORIENTED_EDGE ( 'NONE', *, *, #11493, .F. ) ;
#1249 = ADVANCED_FACE ( 'NONE', ( #27949 ), #10306, .F. ) ;
#1250 = ORIENTED_EDGE ( 'NONE', *, *, #17544, .T. ) ;
#1251 = ORIENTED_EDGE ( 'NONE', *, *, #28136, .T. ) ;
#1252 = CARTESIAN_POINT ( 'NONE',  ( 115.1343022193454146, 230.6109841179907960, 98.75454612047967373 ) ) ;
#1253 = AXIS2_PLACEMENT_3D ( 'NONE', #5028, #2731, #7342 ) ;
#1254 = FACE_OUTER_BOUND ( 'NONE', #3361, .T. ) ;
#1255 = LINE ( 'NONE', #14202, #4246 ) ;
#1256 = VECTOR ( 'NONE', #4847, 1000.000000000000000 ) ;
#1257 = ADVANCED_FACE ( 'NONE', ( #23241 ), #3544, .F. ) ;
#1258 = CARTESIAN_POINT ( 'NONE',  ( -151.7779492149703913, 124.0884682837862556, -18.38425441931939375 ) ) ;
#1259 = CARTESIAN_POINT ( 'NONE',  ( 81.39309752945497678, 249.3891174404998594, -45.00000000000000000 ) ) ;
#1260 = FACE_OUTER_BOUND ( 'NONE', #1079, .T. ) ;
#1261 = LINE ( 'NONE', #14075, #17692 ) ;
#1262 = DIRECTION ( 'NONE',  ( -0.8916010070293584056, -0.4528218681382712996, 0.000000000000000000 ) ) ;
#1263 = CARTESIAN_POINT ( 'NONE',  ( -266.7368518929977768, -170.8180696079899121, -94.49756868224339712 ) ) ;
#1264 = LINE ( 'NONE', #16233, #14272 ) ;
#1265 = CARTESIAN_POINT ( 'NONE',  ( 167.4999999999996589, 526.4263741777961059, 74.99999999999995737 ) ) ;
#1266 = CARTESIAN_POINT ( 'NONE',  ( -200.0000000000000284, -91.18033988749901653, 21.20097097723064294 ) ) ;
#1267 = ORIENTED_EDGE ( 'NONE', *, *, #22908, .T. ) ;
#1268 = EDGE_CURVE ( 'NONE', #17639, #6857, #22211, .T. ) ;
#1269 = CIRCLE ( 'NONE', #23741, 30.00000000000000000 ) ;
#1270 = DIRECTION ( 'NONE',  ( 1.000000000000000000, 0.000000000000000000, 0.000000000000000000 ) ) ;
#1271 = CARTESIAN_POINT ( 'NONE',  ( -195.0490684805821502, 99.44477443395156513, 32.51470260376371613 ) ) ;
#1273 = ORIENTED_EDGE ( 'NONE', *, *, #15927, .F. ) ;
#1272 = ORIENTED_EDGE ( 'NONE', *, *, #22671, .T. ) ;
#1274 = CIRCLE ( 'NONE', #5845, 10.00000000000000888 ) ;
#1275 = ADVANCED_FACE ( 'NONE', ( #6416 ), #19630, .F. ) ;
#1276 = CARTESIAN_POINT ( 'NONE',  ( 157.4999999999998579, 133.4783122410070462, 45.00000000000000000 ) ) ;
#1277 = ORIENTED_EDGE ( 'NONE', *, *, #5268, .T. ) ;
#1278 = ORIENTED_EDGE ( 'NONE', *, *, #5594, .F. ) ;
#1279 = EDGE_LOOP ( 'NONE', ( #24711, #16218, #9881, #10613 ) ) ;
#1280 = ORIENTED_EDGE ( 'NONE', *, *, #8213, .T. ) ;
#1281 = ORIENTED_EDGE ( 'NONE', *, *, #5887, .F. ) ;
#1282 = ORIENTED_EDGE ( 'NONE', *, *, #6019, .F. ) ;
#1283 = DIRECTION ( 'NONE',  ( -1.000000000000000000, 0.000000000000000000, -0.000000000000000000 ) ) ;
#1284 = EDGE_CURVE ( 'NONE', #4946, #19844, #24296, .T. ) ;
#1285 = AXIS2_PLACEMENT_3D ( 'NONE', #5855, #5577, #9897 ) ;
#1286 = EDGE_CURVE ( 'NONE', #7257, #11179, #2231, .T. ) ;
#1287 = VECTOR ( 'NONE', #11569, 1000.000000000000114 ) ;
#1288 = DIRECTION ( 'NONE',  ( 0.000000000000000000, -1.387778780781445429E-16, -1.000000000000000000 ) ) ;
#1289 =( BOUNDED_SURFACE ( )  B_SPLINE_SURFACE ( 3, 2, ( 
 ( #15390, #440, #21979 ),
 ( #2576, #8913, #24144 ),
 ( #297, #22269, #11067 ),
 ( #9054, #19823, #17667 ),
 ( #17808, #24277, #22122 ),
 ( #6892, #15673, #24422 ),
 ( #4731, #13516, #11361 ),
 ( #26712, #15822, #1683 ),
 ( #14914, #2101, #26237 ),
 ( #1819, #10451, #6564 ),
 ( #19636, #28098, #10881 ),
 ( #28373, #23668, #15196 ),
 ( #17055, #27954, #8720 ),
 ( #4262, #25670, #12625 ),
 ( #14770, #4117, #8297 ),
 ( #10311, #25812, #13047 ),
 ( #5993, #23809, #8584 ),
 ( #8442, #17473, #12482 ),
 ( #6139, #17198, #3974 ),
 ( #19070, #12761, #21501 ),
 ( #12902, #28240, #15051 ),
 ( #19209, #10593, #19349 ),
 ( #25956, #15342, #21796 ),
 ( #21363, #23523, #3689 ),
 ( #21222, #6277, #21649 ),
 ( #1545, #27815, #8153 ),
 ( #16914, #1959, #3836 ),
 ( #10742, #19496, #17333 ) ),
 .UNSPECIFIED., .F., .F., .F. ) 
 B_SPLINE_SURFACE_WITH_KNOTS ( ( 4, 2, 2, 2, 2, 2, 2, 2, 2, 2, 2, 2, 2, 4 ),
 ( 3, 3 ),
 ( -4.336808689942017736E-19, 0.002390588749581671821, 0.004781177499163344509, 0.007171766248745017197, 0.009562354998326689018, 0.01434353249749003439, 0.01912470999665337804, 0.02151529874623504812, 0.02390588749581672168, 0.02629647624539839523, 0.02868706499498006879, 0.03346824249414341590, 0.03585883124372508945, 0.03824941999330675607 ),
 ( 0.000000000000000000, 1.000000000000000000 ),
 .UNSPECIFIED. ) 
 GEOMETRIC_REPRESENTATION_ITEM ( )  RATIONAL_B_SPLINE_SURFACE ( (
 ( 1.000000000000000000, 0.9597817246759324794, 1.000000000000000000),
 ( 1.000000000000000000, 0.9562412905049657574, 1.000000000000000000),
 ( 1.000000000000000000, 0.9518158024554053132, 1.000000000000000000),
 ( 1.000000000000000000, 0.9416816922015391889, 1.000000000000000000),
 ( 1.000000000000000000, 0.9359714045868776644, 1.000000000000000000),
 ( 1.000000000000000000, 0.9235548114045784018, 1.000000000000000000),
 ( 1.000000000000000000, 0.9168457509165021113, 1.000000000000000000),
 ( 1.000000000000000000, 0.9026276550354167538, 1.000000000000000000),
 ( 1.000000000000000000, 0.8950913600786598590, 1.000000000000000000),
 ( 1.000000000000000000, 0.8718270562173044969, 1.000000000000000000),
 ( 1.000000000000000000, 0.8553941770535198330, 1.000000000000000000),
 ( 1.000000000000000000, 0.8221312774674292001, 1.000000000000000000),
 ( 1.000000000000000000, 0.8052879325280857259, 1.000000000000000000),
 ( 1.000000000000000000, 0.7809787548410676017, 1.000000000000000000),
 ( 1.000000000000000000, 0.7730264403491060587, 1.000000000000000000),
 ( 1.000000000000000000, 0.7580280365901805872, 1.000000000000000000),
 ( 1.000000000000000000, 0.7509406410103288687, 1.000000000000000000),
 ( 1.000000000000000000, 0.7378319876417124279, 1.000000000000000000),
 ( 1.000000000000000000, 0.7318106482057810114, 1.000000000000000000),
 ( 1.000000000000000000, 0.7210845397427231296, 1.000000000000000000),
 ( 1.000000000000000000, 0.7163689906379826500, 1.000000000000000000),
 ( 1.000000000000000000, 0.7048488289897706371, 1.000000000000000000),
 ( 1.000000000000000000, 0.7005414584674227729, 1.000000000000000000),
 ( 1.000000000000000000, 0.6992757048208856352, 1.000000000000000000),
 ( 1.000000000000000000, 0.6997273220235887825, 1.000000000000000000),
 ( 1.000000000000000000, 0.7022627928042818324, 1.000000000000000000),
 ( 1.000000000000000000, 0.7043340258885323335, 1.000000000000000000),
 ( 1.000000000000000000, 0.7071067811865493491, 1.000000000000000000) ) ) 
 REPRESENTATION_ITEM ( '' )  SURFACE ( )  );
#1290 = LINE ( 'NONE', #16530, #20353 ) ;
#1291 = FACE_BOUND ( 'NONE', #15259, .T. ) ;
#1292 = LINE ( 'NONE', #27842, #24087 ) ;
#1293 = LINE ( 'NONE', #10066, #1770 ) ;
#1294 = CARTESIAN_POINT ( 'NONE',  ( -194.3369914945607491, 63.17511408073718826, -42.65718952139617670 ) ) ;
#1295 = EDGE_CURVE ( 'NONE', #18743, #15118, #13304, .T. ) ;
#1297 = CARTESIAN_POINT ( 'NONE',  ( 112.5172067284654815, 200.1372175834411280, -144.2074248490017681 ) ) ;
#1296 = COLOUR_RGB ( '',0.7921568627450980005, 0.8196078431372548767, 0.9333333333333333481 ) ;
#1298 = LINE ( 'NONE', #23416, #27454 ) ;
#1299 = DIRECTION ( 'NONE',  ( 0.4528218681383106015, 0.8916010070293384215, -0.000000000000000000 ) ) ;
#1300 = FACE_OUTER_BOUND ( 'NONE', #3508, .T. ) ;
#1301 = EDGE_LOOP ( 'NONE', ( #17738, #10843, #12432, #22637 ) ) ;
#1302 = LINE ( 'NONE', #3588, #3177 ) ;
#1303 = EDGE_CURVE ( 'NONE', #26295, #13229, #18628, .T. ) ;
#1304 = AXIS2_PLACEMENT_3D ( 'NONE', #14317, #27788, #3096 ) ;
#1305 = AXIS2_PLACEMENT_3D ( 'NONE', #15444, #19733, #490 ) ;
#1306 = FACE_OUTER_BOUND ( 'NONE', #8945, .T. ) ;
#1307 = EDGE_LOOP ( 'NONE', ( #3003, #20995, #26783, #10191 ) ) ;
#1308 = EDGE_CURVE ( 'NONE', #19372, #18272, #13460, .T. ) ;
#1309 = ORIENTED_EDGE ( 'NONE', *, *, #3636, .T. ) ;
#1310 = ORIENTED_EDGE ( 'NONE', *, *, #17394, .T. ) ;
#1311 = CARTESIAN_POINT ( 'NONE',  ( 100.8904249506254018, 86.57652225510716448, 100.0000000000000142 ) ) ;
#1312 = DIRECTION ( 'NONE',  ( -0.000000000000000000, 0.000000000000000000, 1.000000000000000000 ) ) ;
#1313 = VERTEX_POINT ( 'NONE', #10737 ) ;
#1314 = ORIENTED_EDGE ( 'NONE', *, *, #22173, .F. ) ;
#1315 = CARTESIAN_POINT ( 'NONE',  ( -175.0000000000000000, -150.0000000000000853, 70.00000000000001421 ) ) ;
#1316 = DIRECTION ( 'NONE',  ( 1.000000000000000000, 0.000000000000000000, 0.000000000000000000 ) ) ;
#1317 = CIRCLE ( 'NONE', #14176, 7.685040811306672381 ) ;
#1318 = DIRECTION ( 'NONE',  ( -0.4999999999999865108, 0.8660254037844464792, 0.000000000000000000 ) ) ;
#1320 = EDGE_CURVE ( 'NONE', #6716, #23833, #2515, .T. ) ;
#1319 = ORIENTED_EDGE ( 'NONE', *, *, #26487, .F. ) ;
#1321 = CARTESIAN_POINT ( 'NONE',  ( 96.76194576697650973, 83.89264379418858653, 100.0000000000000142 ) ) ;
#1322 = ORIENTED_EDGE ( 'NONE', *, *, #21568, .T. ) ;
#1323 = DIRECTION ( 'NONE',  ( -1.000000000000000000, 0.000000000000000000, 0.000000000000000000 ) ) ;
#1324 = AXIS2_PLACEMENT_3D ( 'NONE', #25707, #23704, #14811 ) ;
#1325 = AXIS2_PLACEMENT_3D ( 'NONE', #11381, #2888, #5185 ) ;
#1326 = CARTESIAN_POINT ( 'NONE',  ( 6.071532165918828775E-15, -70.00000000000002842, 25.00000000000000000 ) ) ;
#1327 = FACE_OUTER_BOUND ( 'NONE', #26257, .T. ) ;
#1328 = LINE ( 'NONE', #10097, #20457 ) ;
#1329 = CARTESIAN_POINT ( 'NONE',  ( -295.0000000000002274, -157.0000000000000284, -109.9999999999999858 ) ) ;
#1330 = VECTOR ( 'NONE', #18427, 1000.000000000000000 ) ;
#1331 = LINE ( 'NONE', #16710, #7843 ) ;
#1332 = CARTESIAN_POINT ( 'NONE',  ( 162.8938219812283137, 208.9567185848077600, -149.1019530262190642 ) ) ;
#1333 = VERTEX_POINT ( 'NONE', #6835 ) ;
#1334 = PLANE ( 'NONE',  #24695 ) ;
#1335 = DIRECTION ( 'NONE',  ( 0.000000000000000000, 0.000000000000000000, -1.000000000000000000 ) ) ;
#1336 = CARTESIAN_POINT ( 'NONE',  ( 158.0000000000010232, 106.1456246621830957, -45.00000000000000000 ) ) ;
#1337 = DIRECTION ( 'NONE',  ( 0.000000000000000000, -1.000000000000000000, 0.000000000000000000 ) ) ;
#1338 = ORIENTED_EDGE ( 'NONE', *, *, #20073, .T. ) ;
#1339 = EDGE_CURVE ( 'NONE', #6712, #11692, #8855, .T. ) ;
#1340 = DIRECTION ( 'NONE',  ( -0.000000000000000000, -0.000000000000000000, -1.000000000000000000 ) ) ;
#1341 = ADVANCED_FACE ( 'NONE', ( #10873 ), #11018, .F. ) ;
#1342 = VERTEX_POINT ( 'NONE', #15617 ) ;
#1343 = CIRCLE ( 'NONE', #4083, 70.83858790703926900 ) ;
#1344 = CARTESIAN_POINT ( 'NONE',  ( -173.6192398023450494, 113.7611339081862667, 27.04214115208617031 ) ) ;
#1345 = CARTESIAN_POINT ( 'NONE',  ( 130.0130877889311591, 197.5248869502486571, 45.00000000000000000 ) ) ;
#1346 = FACE_OUTER_BOUND ( 'NONE', #4307, .T. ) ;
#1347 = VERTEX_POINT ( 'NONE', #26229 ) ;
#1348 = CARTESIAN_POINT ( 'NONE',  ( -37.82257053376181233, 71.03850157808263077, 100.0000000000000000 ) ) ;
#1349 = VECTOR ( 'NONE', #19200, 1000.000000000000000 ) ;
#1350 = DIRECTION ( 'NONE',  ( 1.000000000000000000, 0.000000000000000000, 0.000000000000000000 ) ) ;
#1351 = ORIENTED_EDGE ( 'NONE', *, *, #1668, .F. ) ;
#1352 = AXIS2_PLACEMENT_3D ( 'NONE', #2714, #11503, #20243 ) ;
#1353 = CARTESIAN_POINT ( 'NONE',  ( 187.4999999999996305, 40.68693696324645970, 45.00000000000000000 ) ) ;
#1354 = CARTESIAN_POINT ( 'NONE',  ( 109.9999999999998721, 259.8688628429572987, 44.77286377382201010 ) ) ;
#1355 = ORIENTED_EDGE ( 'NONE', *, *, #570, .F. ) ;
#1356 = VERTEX_POINT ( 'NONE', #6560 ) ;
#1357 = AXIS2_PLACEMENT_3D ( 'NONE', #25698, #14796, #12504 ) ;
#1358 = CARTESIAN_POINT ( 'NONE',  ( 22.58950924271108107, 154.2349915562422495, -15.00000000000000000 ) ) ;
#1359 = ORIENTED_EDGE ( 'NONE', *, *, #25587, .T. ) ;
#1360 = EDGE_CURVE ( 'NONE', #5793, #19624, #20048, .T. ) ;
#1361 = EDGE_LOOP ( 'NONE', ( #16416, #481, #3606, #1446 ) ) ;
#1362 = VERTEX_POINT ( 'NONE', #24090 ) ;
#1363 = LINE ( 'NONE', #16328, #16208 ) ;
#1364 = CIRCLE ( 'NONE', #18795, 9.999999999999994671 ) ;
#1365 = EDGE_CURVE ( 'NONE', #5280, #14759, #17614, .T. ) ;
#1366 = LINE ( 'NONE', #1775, #8493 ) ;
#1367 = DIRECTION ( 'NONE',  ( 0.8916010070295719014, -0.4528218681378510246, 0.000000000000000000 ) ) ;
#1368 = LINE ( 'NONE', #1645, #8748 ) ;
#1369 = CIRCLE ( 'NONE', #17420, 11.00000000000001066 ) ;
#1370 = DIRECTION ( 'NONE',  ( -0.000000000000000000, -0.000000000000000000, -1.000000000000000000 ) ) ;
#1371 = CARTESIAN_POINT ( 'NONE',  ( 157.9999999999996305, 286.2047501951820436, 45.00000000000000000 ) ) ;
#1372 = LINE ( 'NONE', #25920, #24620 ) ;
#1373 = EDGE_CURVE ( 'NONE', #24637, #27485, #4396, .T. ) ;
#1374 = CARTESIAN_POINT ( 'NONE',  ( 9.999999999999749534, 90.00000000000001421, 98.28427124746191623 ) ) ;
#1375 = CARTESIAN_POINT ( 'NONE',  ( 134.9999999999998295, 537.6859242279716682, -683.1631314933625845 ) ) ;
#1376 = DIRECTION ( 'NONE',  ( -1.000000000000000000, 0.000000000000000000, 0.000000000000000000 ) ) ;
#1377 = ORIENTED_EDGE ( 'NONE', *, *, #15555, .T. ) ;
#1378 = EDGE_CURVE ( 'NONE', #1070, #21067, #12185, .T. ) ;
#1379 = CARTESIAN_POINT ( 'NONE',  ( 0.2652980290584672218, 1.249999999999999778, -7.393354040734018362 ) ) ;
#1380 = EDGE_CURVE ( 'NONE', #2545, #17167, #15192, .T. ) ;
#1381 = CARTESIAN_POINT ( 'NONE',  ( 102.1958639858411004, 244.1335791876568919, -16.70126253799778482 ) ) ;
#1382 = DIRECTION ( 'NONE',  ( 0.8916010070300383061, -0.4528218681369324261, 0.000000000000000000 ) ) ;
#1383 = DIRECTION ( 'NONE',  ( -0.000000000000000000, -0.000000000000000000, -1.000000000000000000 ) ) ;
#1384 = LINE ( 'NONE', #10152, #19373 ) ;
#1385 = ORIENTED_EDGE ( 'NONE', *, *, #24924, .F. ) ;
#1386 = DIRECTION ( 'NONE',  ( -0.9711705445023439687, 0.2383857661250367854, 0.000000000000000000 ) ) ;
#1387 = VERTEX_POINT ( 'NONE', #28234 ) ;
#1388 = CARTESIAN_POINT ( 'NONE',  ( -54.22951502486254327, 83.26691194124390449, -45.00000000000000000 ) ) ;
#1389 = ORIENTED_EDGE ( 'NONE', *, *, #3470, .F. ) ;
#1390 = VERTEX_POINT ( 'NONE', #8577 ) ;
#1391 = CARTESIAN_POINT ( 'NONE',  ( -75.10678314939089262, 136.1130475173332570, 15.20604832699645392 ) ) ;
#1392 = ORIENTED_EDGE ( 'NONE', *, *, #17687, .F. ) ;
#1393 = VERTEX_POINT ( 'NONE', #17329 ) ;
#1394 = CARTESIAN_POINT ( 'NONE',  ( -71.37541315349507443, 240.0000000000000000, -5.000000000000004441 ) ) ;
#1395 = CARTESIAN_POINT ( 'NONE',  ( 79.99999999999990052, 140.0000000000000000, 45.00000000000000000 ) ) ;
#1396 = DIRECTION ( 'NONE',  ( 0.000000000000000000, -1.000000000000000000, 0.000000000000000000 ) ) ;
#1397 = CARTESIAN_POINT ( 'NONE',  ( -135.1444269713557560, 129.7101293712805443, -15.41478258222857001 ) ) ;
#1398 = LINE ( 'NONE', #17195, #2292 ) ;
#1399 = CARTESIAN_POINT ( 'NONE',  ( 157.4999999999998579, 191.1594374136689964, 45.00000000000000000 ) ) ;
#1400 = EDGE_CURVE ( 'NONE', #16387, #24950, #26086, .T. ) ;
#1401 = CARTESIAN_POINT ( 'NONE',  ( -262.3765419278357740, -171.6469950468170111, 89.94932042693801577 ) ) ;
#1402 = VECTOR ( 'NONE', #9107, 1000.000000000000000 ) ;
#1403 = CARTESIAN_POINT ( 'NONE',  ( 129.2024882373296464, 249.4345418698963215, -143.4419542882358485 ) ) ;
#1404 = LINE ( 'NONE', #18932, #21349 ) ;
#1405 = LINE ( 'NONE', #10177, #13351 ) ;
#1406 = CARTESIAN_POINT ( 'NONE',  ( 158.0000000000007390, 135.7322497447605656, 45.00000000000000000 ) ) ;
#1407 = LINE ( 'NONE', #16509, #23066 ) ;
#1408 = ORIENTED_EDGE ( 'NONE', *, *, #26865, .F. ) ;
#1409 = VECTOR ( 'NONE', #10667, 1000.000000000000000 ) ;
#1410 = EDGE_CURVE ( 'NONE', #13433, #14089, #4258, .T. ) ;
#1411 = CARTESIAN_POINT ( 'NONE',  ( -260.0000000000001137, -152.0000000000000284, 60.00000000000002132 ) ) ;
#1413 = ORIENTED_EDGE ( 'NONE', *, *, #22527, .T. ) ;
#1412 = ORIENTED_EDGE ( 'NONE', *, *, #24891, .T. ) ;
#1414 = EDGE_CURVE ( 'NONE', #8004, #24318, #9874, .T. ) ;
#1415 = DIRECTION ( 'NONE',  ( 0.000000000000000000, 1.000000000000000000, 0.000000000000000000 ) ) ;
#1416 = EDGE_LOOP ( 'NONE', ( #15996, #14532, #28328, #12988 ) ) ;
#1417 = ORIENTED_EDGE ( 'NONE', *, *, #15927, .T. ) ;
#1418 = EDGE_LOOP ( 'NONE', ( #12140, #21492, #17241, #7648 ) ) ;
#1419 = VECTOR ( 'NONE', #18095, 1000.000000000000000 ) ;
#1420 = VERTEX_POINT ( 'NONE', #16047 ) ;
#1421 = ORIENTED_EDGE ( 'NONE', *, *, #8652, .T. ) ;
#1422 = EDGE_LOOP ( 'NONE', ( #15865, #11931 ) ) ;
#1423 = DIRECTION ( 'NONE',  ( -0.000000000000000000, 1.000000000000000000, -1.387778780781445429E-16 ) ) ;
#1424 = VECTOR ( 'NONE', #10347, 1000.000000000000000 ) ;
#1425 = CARTESIAN_POINT ( 'NONE',  ( 127.3463313526982716, 201.5224093497739943, 45.00000000000000000 ) ) ;
#1426 = DIRECTION ( 'NONE',  ( -0.8660254037844454800, -0.4999999999999881206, 0.000000000000000000 ) ) ;
#1427 = DIRECTION ( 'NONE',  ( -0.000000000000000000, -0.000000000000000000, -1.000000000000000000 ) ) ;
#1428 = EDGE_CURVE ( 'NONE', #11694, #24469, #24800, .T. ) ;
#1429 = CARTESIAN_POINT ( 'NONE',  ( -279.1278187736259611, -165.0000000000001137, -106.1966075482097978 ) ) ;
#1430 = DIRECTION ( 'NONE',  ( 0.000000000000000000, -1.000000000000000000, 0.000000000000000000 ) ) ;
#1431 = DIRECTION ( 'NONE',  ( -0.000000000000000000, -0.000000000000000000, -1.000000000000000000 ) ) ;
#1432 = AXIS2_PLACEMENT_3D ( 'NONE', #1964, #14773, #18933 ) ;
#1433 = CARTESIAN_POINT ( 'NONE',  ( 110.3467068720617590, 202.9047393083059205, -139.5322470298331439 ) ) ;
#1434 = LINE ( 'NONE', #10346, #2698 ) ;
#1435 = PLANE ( 'NONE',  #17938 ) ;
#1436 = LINE ( 'NONE', #20978, #10652 ) ;
#1437 = ORIENTED_EDGE ( 'NONE', *, *, #22794, .T. ) ;
#1438 = VECTOR ( 'NONE', #8418, 1000.000000000000000 ) ;
#1439 = LINE ( 'NONE', #20844, #20621 ) ;
#1440 = VECTOR ( 'NONE', #10465, 1000.000000000000000 ) ;
#1441 = EDGE_CURVE ( 'NONE', #27071, #21404, #16329, .T. ) ;
#1442 = EDGE_CURVE ( 'NONE', #13173, #17645, #9851, .T. ) ;
#1443 = CARTESIAN_POINT ( 'NONE',  ( -40.40953891503691153, 36.92584315232891612, 99.00000000000000000 ) ) ;
#1444 = VERTEX_POINT ( 'NONE', #7129 ) ;
#1445 = DIRECTION ( 'NONE',  ( 0.000000000000000000, 0.000000000000000000, 1.000000000000000000 ) ) ;
#1446 = ORIENTED_EDGE ( 'NONE', *, *, #16888, .T. ) ;
#1447 = ORIENTED_EDGE ( 'NONE', *, *, #1879, .F. ) ;
#1448 = CARTESIAN_POINT ( 'NONE',  ( 90.92319367350451387, 112.0484670279762440, 100.0000000000108429 ) ) ;
#1449 = LINE ( 'NONE', #22871, #12208 ) ;
#1450 = ORIENTED_EDGE ( 'NONE', *, *, #24142, .F. ) ;
#1452 = EDGE_CURVE ( 'NONE', #24464, #6433, #3888, .T. ) ;
#1451 = EDGE_LOOP ( 'NONE', ( #18837, #7191, #7969 ) ) ;
#1453 = DIRECTION ( 'NONE',  ( 0.4528218681382713551, 0.8916010070293584056, -0.000000000000000000 ) ) ;
#1454 = EDGE_CURVE ( 'NONE', #6404, #25224, #9712, .T. ) ;
#1455 = VECTOR ( 'NONE', #19141, 1000.000000000000000 ) ;
#1456 = DIRECTION ( 'NONE',  ( -0.000000000000000000, -0.000000000000000000, -1.000000000000000000 ) ) ;
#1457 = CARTESIAN_POINT ( 'NONE',  ( -180.5998324953250176, 109.6502091928870328, -29.97430207196073937 ) ) ;
#1458 = ORIENTED_EDGE ( 'NONE', *, *, #9523, .F. ) ;
#1459 = DIRECTION ( 'NONE',  ( 0.9239321509641974517, 1.061807240666843741E-15, 0.3825563754725196941 ) ) ;
#1460 = VERTEX_POINT ( 'NONE', #9437 ) ;
#1461 = VECTOR ( 'NONE', #24885, 1000.000000000000000 ) ;
#1462 = AXIS2_PLACEMENT_3D ( 'NONE', #18831, #889, #27438 ) ;
#1463 = CARTESIAN_POINT ( 'NONE',  ( -68.57415822541635464, 29.64876300893806516, 95.00000000000000000 ) ) ;
#1464 = MECHANICAL_DESIGN_GEOMETRIC_PRESENTATION_REPRESENTATION (  '', ( #27159 ), #20745 ) ;
#1465 = DIRECTION ( 'NONE',  ( 0.8916010070297547552, 0.4528218681374907018, 0.000000000000000000 ) ) ;
#1466 = EDGE_CURVE ( 'NONE', #27470, #21163, #18610, .T. ) ;
#1467 = PLANE ( 'NONE',  #6625 ) ;
#1468 = PLANE ( 'NONE',  #18635 ) ;
#1469 = DIRECTION ( 'NONE',  ( -1.321694076934710155E-16, 1.000000000000000000, 0.000000000000000000 ) ) ;
#1470 = CARTESIAN_POINT ( 'NONE',  ( 179.9999999999999147, 526.4263741777961059, 84.99999999999997158 ) ) ;
#1471 = CARTESIAN_POINT ( 'NONE',  ( 163.1912130698789554, 209.7382084964983733, -148.0040471605078380 ) ) ;
#1472 = EDGE_LOOP ( 'NONE', ( #27900, #5923 ) ) ;
#1473 = DIRECTION ( 'NONE',  ( 1.000000000000000000, -0.000000000000000000, -0.000000000000000000 ) ) ;
#1474 = DIRECTION ( 'NONE',  ( -0.8916010070298258094, -0.4528218681373508137, 0.000000000000000000 ) ) ;
#1475 = CARTESIAN_POINT ( 'NONE',  ( 282.4999999999996589, 19.41075299063184900, 87.99671038392668265 ) ) ;
#1476 = CYLINDRICAL_SURFACE ( 'NONE', #6613, 5.999999999999991118 ) ;
#1477 = ORIENTED_EDGE ( 'NONE', *, *, #23081, .F. ) ;
#1478 = VECTOR ( 'NONE', #2911, 1000.000000000000114 ) ;
#1479 = DIRECTION ( 'NONE',  ( 1.000000000000000000, -0.000000000000000000, -0.000000000000000000 ) ) ;
#1480 = VERTEX_POINT ( 'NONE', #7274 ) ;
#1481 = CIRCLE ( 'NONE', #11600, 16.07743405327025243 ) ;
#1482 = CARTESIAN_POINT ( 'NONE',  ( -191.5126735617889437, 102.3039448627891659, 32.04604572034998711 ) ) ;
#1483 = DIRECTION ( 'NONE',  ( -0.000000000000000000, -0.000000000000000000, -1.000000000000000000 ) ) ;
#1484 = DIRECTION ( 'NONE',  ( 0.000000000000000000, 1.214306433183764720E-16, -1.000000000000000000 ) ) ;
#1485 = ORIENTED_EDGE ( 'NONE', *, *, #25059, .F. ) ;
#1486 = FACE_OUTER_BOUND ( 'NONE', #5203, .T. ) ;
#1487 = LINE ( 'NONE', #27761, #26260 ) ;
#1488 = CIRCLE ( 'NONE', #16191, 10.71881775658151170 ) ;
#1489 = ORIENTED_EDGE ( 'NONE', *, *, #27303, .F. ) ;
#1490 = VECTOR ( 'NONE', #17807, 1000.000000000000000 ) ;
#1491 = LINE ( 'NONE', #19440, #19816 ) ;
#1492 = CARTESIAN_POINT ( 'NONE',  ( 109.9579984081460680, 258.6776769496694897, 42.70939860559244750 ) ) ;
#1493 = VERTEX_POINT ( 'NONE', #18474 ) ;
#1494 = ORIENTED_EDGE ( 'NONE', *, *, #12522, .F. ) ;
#1495 = CARTESIAN_POINT ( 'NONE',  ( -210.0000000000000568, -220.0000000000000853, -109.1217062362807155 ) ) ;
#1496 = ORIENTED_EDGE ( 'NONE', *, *, #26575, .T. ) ;
#1497 = EDGE_LOOP ( 'NONE', ( #15130, #928, #10438, #25905 ) ) ;
#1498 = ORIENTED_EDGE ( 'NONE', *, *, #13064, .T. ) ;
#1499 = AXIS2_PLACEMENT_3D ( 'NONE', #7927, #16556, #3745 ) ;
#1500 = LINE ( 'NONE', #14726, #16224 ) ;
#1501 = ADVANCED_FACE ( 'NONE', ( #26947 ), #11741, .F. ) ;
#1502 = VECTOR ( 'NONE', #13508, 1000.000000000000000 ) ;
#1503 = CARTESIAN_POINT ( 'NONE',  ( 158.0000000000012506, 88.08262460212675649, 45.00000000000000000 ) ) ;
#1504 = ADVANCED_FACE ( 'NONE', ( #27224 ), #17208, .T. ) ;
#1505 = LINE ( 'NONE', #25358, #23863 ) ;
#1506 = TOROIDAL_SURFACE ( 'NONE', #27199, 7.108535549237485540, 0.4000000000000000222 ) ;
#1507 = VECTOR ( 'NONE', #23226, 1000.000000000000000 ) ;
#1508 = DIRECTION ( 'NONE',  ( -1.321694076934710155E-16, 1.000000000000000000, 0.000000000000000000 ) ) ;
#1509 = CARTESIAN_POINT ( 'NONE',  ( 157.4999999999998579, 158.5570623160774630, -45.00000000000000000 ) ) ;
#1510 = CARTESIAN_POINT ( 'NONE',  ( -237.0233935005625483, 68.72940251376158471, -14.95240471282613193 ) ) ;
#1511 = LINE ( 'NONE', #14593, #11785 ) ;
#1512 = LINE ( 'NONE', #3944, #4648 ) ;
#1513 = DIRECTION ( 'NONE',  ( -0.000000000000000000, -0.000000000000000000, 1.000000000000000000 ) ) ;
#1514 = CARTESIAN_POINT ( 'NONE',  ( 112.5174913703661446, 218.9750123000742121, -96.63436734148044138 ) ) ;
#1515 = VERTEX_POINT ( 'NONE', #3229 ) ;
#1516 = CARTESIAN_POINT ( 'NONE',  ( 232.4999999999996305, 133.0668745871126930, -36.86484227207694886 ) ) ;
#1517 = DIRECTION ( 'NONE',  ( 0.4528218681383106015, 0.8916010070293384215, -0.000000000000000000 ) ) ;
#1518 = CARTESIAN_POINT ( 'NONE',  ( 12.09558415809990883, 89.94522053857441790, 98.30381960812032105 ) ) ;
#1519 = CARTESIAN_POINT ( 'NONE',  ( -160.0000000000000284, 59.99999999999994316, 100.0000000000000142 ) ) ;
#1520 = DIRECTION ( 'NONE',  ( -1.850371707708594316E-16, 1.000000000000000000, 0.000000000000000000 ) ) ;
#1521 = ORIENTED_EDGE ( 'NONE', *, *, #20800, .F. ) ;
#1522 = VECTOR ( 'NONE', #12404, 1000.000000000000000 ) ;
#1523 = CIRCLE ( 'NONE', #17573, 1.000000000000000888 ) ;
#1524 = CARTESIAN_POINT ( 'NONE',  ( -17.24491960465745777, -18.01420295945611727, 95.00000000000000000 ) ) ;
#1525 = ORIENTED_EDGE ( 'NONE', *, *, #23009, .F. ) ;
#1526 = ADVANCED_FACE ( 'NONE', ( #5388 ), #5107, .F. ) ;
#1527 = DIRECTION ( 'NONE',  ( 1.000000000000000000, -0.000000000000000000, -0.000000000000000000 ) ) ;
#1528 = VERTEX_POINT ( 'NONE', #24940 ) ;
#1529 = VECTOR ( 'NONE', #5297, 1000.000000000000000 ) ;
#1530 = ORIENTED_EDGE ( 'NONE', *, *, #23337, .F. ) ;
#1531 = LINE ( 'NONE', #10581, #12226 ) ;
#1532 = EDGE_LOOP ( 'NONE', ( #1222, #7249, #21467, #6614 ) ) ;
#1533 = EDGE_CURVE ( 'NONE', #27544, #6317, #524, .T. ) ;
#1534 = VERTEX_POINT ( 'NONE', #14171 ) ;
#1535 = CARTESIAN_POINT ( 'NONE',  ( 112.5712424644273426, 217.9445819143301435, 96.69730840357098600 ) ) ;
#1536 = CARTESIAN_POINT ( 'NONE',  ( -157.8051893169759126, 120.7082176335777177, -21.99009546054191944 ) ) ;
#1537 = DIRECTION ( 'NONE',  ( 0.8916010070296530587, 0.4528218681376912080, 0.000000000000000000 ) ) ;
#1538 = EDGE_CURVE ( 'NONE', #13911, #7659, #15377, .T. ) ;
#1539 = EDGE_CURVE ( 'NONE', #18389, #14865, #22924, .T. ) ;
#1540 = EDGE_CURVE ( 'NONE', #2445, #22920, #20876, .T. ) ;
#1541 = LINE ( 'NONE', #19065, #27950 ) ;
#1542 = CARTESIAN_POINT ( 'NONE',  ( 232.4999999999996305, 133.0668745871126930, -30.83984227207694317 ) ) ;
#1543 = DIRECTION ( 'NONE',  ( 1.000000000000000000, 0.000000000000000000, 0.000000000000000000 ) ) ;
#1544 = CARTESIAN_POINT ( 'NONE',  ( 24.17452580132986739, -46.52307359567973322, 99.29556765389919804 ) ) ;
#1545 = CARTESIAN_POINT ( 'NONE',  ( -232.1637141486664575, 91.03144149473433799, -15.02585134956874668 ) ) ;
#1546 = VECTOR ( 'NONE', #16501, 1000.000000000000000 ) ;
#1547 = PRODUCT ( 'slotted cheese head screw_iso_ISO 1207 - M10 x 35 - 35N', 'slotted cheese head screw_iso_ISO 1207 - M10 x 35 - 35N', '', ( #10217 ) ) ;
#1548 = DIRECTION ( 'NONE',  ( 0.000000000000000000, 0.5150380749100555988, 0.8571673007021114454 ) ) ;
#1549 = CARTESIAN_POINT ( 'NONE',  ( -232.1720359504865883, 90.98239771430922929, 14.99999999999994849 ) ) ;
#1550 = VECTOR ( 'NONE', #20732, 1000.000000000000000 ) ;
#1551 = DIRECTION ( 'NONE',  ( 0.2066290158914464714, -0.9784193629480829602, 0.000000000000000000 ) ) ;
#1552 = DIRECTION ( 'NONE',  ( 0.000000000000000000, 0.000000000000000000, 1.000000000000000000 ) ) ;
#1553 = DIRECTION ( 'NONE',  ( -0.000000000000000000, -0.000000000000000000, -1.000000000000000000 ) ) ;
#1554 = VERTEX_POINT ( 'NONE', #1084 ) ;
#1555 = PLANE ( 'NONE',  #27926 ) ;
#1556 = CARTESIAN_POINT ( 'NONE',  ( 106.6702556437889484, 210.1292660578155562, -147.1195141158910360 ) ) ;
#1558 = ORIENTED_EDGE ( 'NONE', *, *, #24325, .F. ) ;
#1557 = ORIENTED_EDGE ( 'NONE', *, *, #9327, .F. ) ;
#1559 = CARTESIAN_POINT ( 'NONE',  ( 98.16608178754364644, 241.2913188899317163, -20.91842009986573814 ) ) ;
#1560 = ORIENTED_EDGE ( 'NONE', *, *, #25133, .T. ) ;
#1561 = ORIENTED_EDGE ( 'NONE', *, *, #19792, .F. ) ;
#1562 = ORIENTED_EDGE ( 'NONE', *, *, #20866, .T. ) ;
#1563 = EDGE_CURVE ( 'NONE', #10183, #19021, #8058, .T. ) ;
#1564 = EDGE_CURVE ( 'NONE', #18588, #18031, #10134, .T. ) ;
#1565 = ORIENTED_EDGE ( 'NONE', *, *, #148, .T. ) ;
#1566 = VECTOR ( 'NONE', #4191, 1000.000000000000000 ) ;
#1567 = EDGE_LOOP ( 'NONE', ( #19464, #20883, #3429, #20222 ) ) ;
#1568 = VERTEX_POINT ( 'NONE', #14449 ) ;
#1569 = DIRECTION ( 'NONE',  ( -0.7348549764921098459, 0.6782242722910915012, 4.000673683678708817E-14 ) ) ;
#1570 = EDGE_CURVE ( 'NONE', #9462, #6741, #17622, .T. ) ;
#1571 = EDGE_CURVE ( 'NONE', #11251, #16161, #1366, .T. ) ;
#1572 = CARTESIAN_POINT ( 'NONE',  ( -225.7036482868739427, -91.18033988749901653, 0.000000000000000000 ) ) ;
#1573 = CARTESIAN_POINT ( 'NONE',  ( 158.0000000000017337, 42.94087446699998623, 45.00000000000000000 ) ) ;
#1574 = PRODUCT_RELATED_PRODUCT_CATEGORY ( 'part', '', ( #1547 ) ) ;
#1575 = FACE_OUTER_BOUND ( 'NONE', #10297, .T. ) ;
#1576 = PLANE ( 'NONE',  #17380 ) ;
#1577 = CARTESIAN_POINT ( 'NONE',  ( -216.5430934856041745, 71.49318776575898937, -24.90892144430478794 ) ) ;
#1578 = CONICAL_SURFACE ( 'NONE', #213, 5.999999999999977796, 1.029744258676652979 ) ;
#1579 = FACE_OUTER_BOUND ( 'NONE', #10470, .T. ) ;
#1580 = CARTESIAN_POINT ( 'NONE',  ( -68.97958094182604327, 102.2323340340523288, -162.9307281190808681 ) ) ;
#1581 = CARTESIAN_POINT ( 'NONE',  ( 158.0000000000004547, 165.8267498348450886, 45.00000000000000000 ) ) ;
#1582 = DIRECTION ( 'NONE',  ( -0.000000000000000000, -0.000000000000000000, -1.000000000000000000 ) ) ;
#1583 = TOROIDAL_SURFACE ( 'NONE', #22239, 45.00000000000000711, 5.000000000000000000 ) ;
#1584 = ORIENTED_EDGE ( 'NONE', *, *, #16537, .F. ) ;
#1585 = DIRECTION ( 'NONE',  ( -0.000000000000000000, -0.000000000000000000, -1.000000000000000000 ) ) ;
#1586 = FACE_OUTER_BOUND ( 'NONE', #20704, .T. ) ;
#1587 = ORIENTED_EDGE ( 'NONE', *, *, #169, .F. ) ;
#1588 = ORIENTED_EDGE ( 'NONE', *, *, #16351, .F. ) ;
#1589 = ORIENTED_EDGE ( 'NONE', *, *, #23458, .F. ) ;
#1590 = EDGE_CURVE ( 'NONE', #16800, #27270, #27778, .T. ) ;
#1591 = DIRECTION ( 'NONE',  ( 0.4528218681372521703, 0.8916010070298759915, -0.000000000000000000 ) ) ;
#1592 = DIRECTION ( 'NONE',  ( -0.8916010070294808632, -0.4528218681380302146, 0.000000000000000000 ) ) ;
#1593 = ORIENTED_EDGE ( 'NONE', *, *, #22913, .T. ) ;
#1594 = AXIS2_PLACEMENT_3D ( 'NONE', #11454, #27087, #16189 ) ;
#1595 = CIRCLE ( 'NONE', #25913, 30.00000000000000000 ) ;
#1596 = ORIENTED_EDGE ( 'NONE', *, *, #15234, .T. ) ;
#1597 = CARTESIAN_POINT ( 'NONE',  ( 157.9999999999997726, 243.5708750675630370, -45.00000000000000000 ) ) ;
#1598 = CARTESIAN_POINT ( 'NONE',  ( 157.4999999999998579, 65.76568703831686946, 45.00000000000000000 ) ) ;
#1599 = DIRECTION ( 'NONE',  ( -0.8916010070297953893, -0.4528218681374107657, 0.000000000000000000 ) ) ;
#1600 = VERTEX_POINT ( 'NONE', #14308 ) ;
#1601 = CARTESIAN_POINT ( 'NONE',  ( 95.20156243614241021, 83.09913198708241566, 100.0000000000000142 ) ) ;
#1602 = VERTEX_POINT ( 'NONE', #25629 ) ;
#1603 = CIRCLE ( 'NONE', #25453, 5.000000000000004441 ) ;
#1604 = FACE_OUTER_BOUND ( 'NONE', #3933, .T. ) ;
#1605 = EDGE_CURVE ( 'NONE', #1132, #25965, #23343, .T. ) ;
#1606 = PLANE ( 'NONE',  #14436 ) ;
#1607 = DIRECTION ( 'NONE',  ( 1.000000000000000000, 0.000000000000000000, 0.000000000000000000 ) ) ;
#1608 = PLANE ( 'NONE',  #17319 ) ;
#1609 = DIRECTION ( 'NONE',  ( -0.7082136108520787898, -0.7059982162894324897, -0.000000000000000000 ) ) ;
#1610 = CARTESIAN_POINT ( 'NONE',  ( 163.4054721189930035, 210.3495760014581606, -143.6319245046324511 ) ) ;
#1611 = ORIENTED_EDGE ( 'NONE', *, *, #3192, .T. ) ;
#1612 = CARTESIAN_POINT ( 'NONE',  ( 158.0000000000014211, 71.03537455708449500, 45.00000000000000000 ) ) ;
#1613 = PLANE ( 'NONE',  #28005 ) ;
#1614 = PLANE ( 'NONE',  #24868 ) ;
#1615 = LINE ( 'NONE', #19142, #16708 ) ;
#1616 = EDGE_LOOP ( 'NONE', ( #18989, #23428, #19375, #25548 ) ) ;
#1617 = AXIS2_PLACEMENT_3D ( 'NONE', #5431, #16231, #11784 ) ;
#1618 = EDGE_CURVE ( 'NONE', #16979, #5099, #5678, .T. ) ;
#1619 = LINE ( 'NONE', #23740, #6834 ) ;
#1620 = EDGE_CURVE ( 'NONE', #28289, #17098, #27637, .T. ) ;
#1621 = CARTESIAN_POINT ( 'NONE',  ( 147.1752285801744904, 204.1329331941753082, -45.00000000000000000 ) ) ;
#1622 = DIRECTION ( 'NONE',  ( 1.000000000000000000, 0.000000000000000000, 0.000000000000000000 ) ) ;
#1623 = DIRECTION ( 'NONE',  ( 0.000000000000000000, 0.000000000000000000, -1.000000000000000000 ) ) ;
#1624 = ORIENTED_EDGE ( 'NONE', *, *, #10974, .T. ) ;
#1625 = DIRECTION ( 'NONE',  ( 1.000000000000000000, 0.000000000000000000, 0.000000000000000000 ) ) ;
#1626 = PLANE ( 'NONE',  #24440 ) ;
#1627 = VECTOR ( 'NONE', #17436, 1000.000000000000000 ) ;
#1628 = EDGE_LOOP ( 'NONE', ( #28305, #27759, #13384, #15254 ) ) ;
#1629 = DIRECTION ( 'NONE',  ( -0.000000000000000000, -0.000000000000000000, -1.000000000000000000 ) ) ;
#1630 = DIRECTION ( 'NONE',  ( 0.000000000000000000, 0.000000000000000000, -1.000000000000000000 ) ) ;
#1631 = ORIENTED_EDGE ( 'NONE', *, *, #5242, .F. ) ;
#1632 = ORIENTED_EDGE ( 'NONE', *, *, #5428, .T. ) ;
#1633 = LINE ( 'NONE', #10545, #15004 ) ;
#1634 = ORIENTED_EDGE ( 'NONE', *, *, #22159, .T. ) ;
#1635 = AXIS2_PLACEMENT_3D ( 'NONE', #16913, #25532, #23808 ) ;
#1636 = ORIENTED_EDGE ( 'NONE', *, *, #26899, .F. ) ;
#1637 = VERTEX_POINT ( 'NONE', #23622 ) ;
#1638 = AXIS2_PLACEMENT_3D ( 'NONE', #16135, #26603, #15998 ) ;
#1639 = CARTESIAN_POINT ( 'NONE',  ( 157.9999999999996305, 281.6968751876750616, 45.00000000000000000 ) ) ;
#1640 = EDGE_CURVE ( 'NONE', #13707, #5522, #3935, .T. ) ;
#1641 = EDGE_CURVE ( 'NONE', #5984, #20120, #8115, .T. ) ;
#1642 = DIRECTION ( 'NONE',  ( 0.8916010070299374979, 0.4528218681371309895, 0.000000000000000000 ) ) ;
#1643 = CARTESIAN_POINT ( 'NONE',  ( 0.6945804017089570737, 136.6086003902396158, 13.39232072666088769 ) ) ;
#1644 = DIRECTION ( 'NONE',  ( 0.000000000000000000, 0.000000000000000000, -1.000000000000000000 ) ) ;
#1645 = CARTESIAN_POINT ( 'NONE',  ( -210.0000000000000568, -220.0000000000000853, -89.99999999999987210 ) ) ;
#1646 = CARTESIAN_POINT ( 'NONE',  ( 209.9999999999999432, -150.0000000000000284, -99.99999999999995737 ) ) ;
#1647 = CARTESIAN_POINT ( 'NONE',  ( -232.3018049223840364, 76.77033509348976281, -15.55816966298101178 ) ) ;
#1648 = ORIENTED_EDGE ( 'NONE', *, *, #22288, .T. ) ;
#1649 = DIRECTION ( 'NONE',  ( 1.000000000000000000, 0.000000000000000000, 0.000000000000000000 ) ) ;
#1650 = CARTESIAN_POINT ( 'NONE',  ( 177.1897033089359184, 197.3087408678716770, 45.00000000000000000 ) ) ;
#1651 = CARTESIAN_POINT ( 'NONE',  ( -248.1546605714623013, -91.18033988749901653, 16.91094714394370158 ) ) ;
#1652 = CARTESIAN_POINT ( 'NONE',  ( 158.0000000000000853, 198.4291249324366504, -45.00000000000000000 ) ) ;
#1653 = VERTEX_POINT ( 'NONE', #12442 ) ;
#1654 = EDGE_CURVE ( 'NONE', #3789, #4321, #7583, .T. ) ;
#1655 = CARTESIAN_POINT ( 'NONE',  ( -210.0000000000000568, -157.0000000000000284, 90.00000000000002842 ) ) ;
#1656 = CARTESIAN_POINT ( 'NONE',  ( 134.9999999999998579, 220.0000000000000284, 109.9999999999999858 ) ) ;
#1657 = CARTESIAN_POINT ( 'NONE',  ( 96.24933711586670881, 240.9969687801728639, -9.998578604269592773 ) ) ;
#1658 = DIRECTION ( 'NONE',  ( -0.000000000000000000, -0.000000000000000000, 1.000000000000000000 ) ) ;
#1659 = CYLINDRICAL_SURFACE ( 'NONE', #24420, 5.000000000000004441 ) ;
#1660 = ORIENTED_EDGE ( 'NONE', *, *, #12229, .T. ) ;
#1662 = EDGE_CURVE ( 'NONE', #14427, #8519, #11250, .T. ) ;
#1661 = VECTOR ( 'NONE', #17745, 1000.000000000000000 ) ;
#1663 = ADVANCED_FACE ( 'NONE', ( #12583 ), #27911, .F. ) ;
#1664 = LINE ( 'NONE', #21342, #1954 ) ;
#1665 = ORIENTED_EDGE ( 'NONE', *, *, #26664, .F. ) ;
#1666 = DIRECTION ( 'NONE',  ( -0.9784193629480785193, 0.2066290158914672603, 0.000000000000000000 ) ) ;
#1667 = ORIENTED_EDGE ( 'NONE', *, *, #9784, .T. ) ;
#1668 = EDGE_CURVE ( 'NONE', #12610, #1602, #6094, .T. ) ;
#1669 = VECTOR ( 'NONE', #26953, 1000.000000000000000 ) ;
#1670 = VERTEX_POINT ( 'NONE', #14875 ) ;
#1671 = FACE_OUTER_BOUND ( 'NONE', #20428, .T. ) ;
#1672 = ORIENTED_EDGE ( 'NONE', *, *, #24020, .T. ) ;
#1673 = EDGE_LOOP ( 'NONE', ( #5843, #13373 ) ) ;
#1674 = DIRECTION ( 'NONE',  ( 0.000000000000000000, 0.000000000000000000, 1.000000000000000000 ) ) ;
#1675 = FACE_BOUND ( 'NONE', #2044, .T. ) ;
#1676 = DIRECTION ( 'NONE',  ( 0.8660254037844432595, 0.4999999999999919509, -0.000000000000000000 ) ) ;
#1677 = CARTESIAN_POINT ( 'NONE',  ( -158.6398931503276515, 121.2395900921240610, -20.46722486591957946 ) ) ;
#1678 = ADVANCED_FACE ( 'NONE', ( #28054 ), #10553, .F. ) ;
#1679 = AXIS2_PLACEMENT_3D ( 'NONE', #10968, #21595, #28047 ) ;
#1680 = LINE ( 'NONE', #10448, #20191 ) ;
#1681 = DIRECTION ( 'NONE',  ( 0.8916010070297745171, -0.4528218681374519550, 0.000000000000000000 ) ) ;
#1682 = CARTESIAN_POINT ( 'NONE',  ( 31.66302550918311809, -40.78000118157726916, 100.0000000000000000 ) ) ;
#1683 = CARTESIAN_POINT ( 'NONE',  ( -208.4928213732883080, 89.66777255638292843, -24.75805542544560112 ) ) ;
#1684 = DIRECTION ( 'NONE',  ( 1.000000000000000000, 0.000000000000000000, -0.000000000000000000 ) ) ;
#1685 = CARTESIAN_POINT ( 'NONE',  ( 157.9999999999997442, 253.6023750975910502, -45.00000000000000000 ) ) ;
#1686 = CARTESIAN_POINT ( 'NONE',  ( -20.92338318254765994, 120.7399884395670142, -145.0000000000000000 ) ) ;
#1687 = FACE_BOUND ( 'NONE', #7272, .T. ) ;
#1688 = DIRECTION ( 'NONE',  ( -0.000000000000000000, -0.000000000000000000, -1.000000000000000000 ) ) ;
#1689 = ORIENTED_EDGE ( 'NONE', *, *, #11782, .T. ) ;
#1690 = DIRECTION ( 'NONE',  ( 0.8916010070293283185, 0.4528218681383305855, 0.000000000000000000 ) ) ;
#1691 = LINE ( 'NONE', #13060, #21313 ) ;
#1692 = CARTESIAN_POINT ( 'NONE',  ( 108.3633886251205638, 206.1968162351656986, -150.8460904732142183 ) ) ;
#1694 = ORIENTED_EDGE ( 'NONE', *, *, #19190, .F. ) ;
#1693 = ORIENTED_EDGE ( 'NONE', *, *, #14822, .F. ) ;
#1695 = EDGE_CURVE ( 'NONE', #7257, #2661, #23650, .T. ) ;
#1696 = ADVANCED_FACE ( 'NONE', ( #27494 ), #7832, .T. ) ;
#1697 = CARTESIAN_POINT ( 'NONE',  ( 93.32984351717588822, 231.0185867901169274, -18.11991709984777188 ) ) ;
#1698 = ORIENTED_EDGE ( 'NONE', *, *, #3838, .T. ) ;
#1699 = ORIENTED_EDGE ( 'NONE', *, *, #2899, .F. ) ;
#1700 = AXIS2_PLACEMENT_3D ( 'NONE', #16971, #14830, #16696 ) ;
#1701 = ORIENTED_EDGE ( 'NONE', *, *, #1570, .T. ) ;
#1702 = CLOSED_SHELL ( 'NONE', ( #5037, #14678, #23234, #5502, #24283, #14938, #2265, #6554, #3871, #2199, #13933, #9365, #2896, #4437, #25882, #26524, #5267, #4378, #12675, #6374, #8968, #4779, #26328, #344, #6068, #9450, #12969, #18762, #20514, #6727, #1875, #10853, #18742, #5392, #13194, #12582, #19277, #18166, #19085, #10440, #18221, #18566, #25618, #12253, #14647, #10464, #17080, #19475, #15268, #9869, #23580, #6182, #21632, #24409, #1526, #6628, #10736, #19240, #3927, #7253, #24780, #18626, #19478, #24983, #23988, #16736, #15592, #10260, #23262, #15724, #26552, #13560, #22249, #180, #22593, #10691, #3798, #23786, #25039, #26910, #4809, #21961, #7831, #14753, #24354, #19010, #19761, #17454, #20021, #7354, #8581, #19145, #314, #2624, #8857, #25494, #939, #25019, #9129, #2966, #27152, #26925, #14259, #12894, #3707, #12651, #19439, #10937, #17272, #5615, #22983, #19660, #26651, #10955, #27873, #5324, #1915, #28026, #21153, #11826, #13205, #6460, #11114, #9036, #18486, #25249, #11745, #7152, #18596, #28329, #25125, #16182, #19441, #16215, #22230, #8313, #15900, #15073, #8508, #9344, #1243, #3247, #25582, #7338, #20421, #23414, #15097, #3922, #13722, #23619, #25027, #1178, #10674, #6214, #9098, #17169, #2398, #14100, #12721, #17965, #5525, #28323, #510, #15748, #26744, #9981, #6234, #23359, #13048, #1044, #6299, #224, #21750, #3083, #21148, #22875, #25886, #15159, #19007, #1057, #6980, #2584, #26022, #4016, #22674, #7351, #21783, #27274, #4794, #17226, #19758, #21928, #27153, #4612, #19467, #13247, #5694, #9082, #9434, #19499, #4868, #25515, #1257, #26488, #26113, #4151, #26822, #3805, #10457, #4468, #21309, #4634, #14273, #21906, #1016, #28194, #8459, #4106, #1109, #5454, #7777, #12803, #2308, #15557, #7607, #2112, #15237, #23165, #3246, #8094, #19637, #13237, #26392, #24327, #27246, #4082, #14612, #27495, #4346, #17624, #20076, #17132, #18759, #6232, #9507, #18288, #2132, #10414, #7489, #27770, #3054, #4015, #20011, #26666, #24896, #16228, #15401, #4271, #21454, #2267, #6874, #23913, #8462, #15657, #3665, #23687, #14364, #4337, #24772, #22826, #21896, #3302, #22051, #25792, #27461, #16196, #17007, #744, #25723, #17686, #20797, #16970, #1663, #24481, #27557, #6400, #25152, #23760, #16430, #25953, #7550, #12743, #21257, #9536, #28213, #16597, #25935, #5106, #24730, #5420, #4153, #2602, #18380, #9162, #15369, #14626 ) ) ;
#1703 = ORIENTED_EDGE ( 'NONE', *, *, #14809, .T. ) ;
#1704 = ORIENTED_EDGE ( 'NONE', *, *, #7266, .T. ) ;
#1705 = ORIENTED_EDGE ( 'NONE', *, *, #12376, .F. ) ;
#1706 = DIRECTION ( 'NONE',  ( 0.8916010070295207202, -0.4528218681379515553, 0.000000000000000000 ) ) ;
#1707 = CARTESIAN_POINT ( 'NONE',  ( 144.9999999999998863, 220.0000000000000284, -45.00000000000000000 ) ) ;
#1708 = CARTESIAN_POINT ( 'NONE',  ( -138.6428522700808230, 71.54464929955099706, 80.00000000000001421 ) ) ;
#1709 = DIRECTION ( 'NONE',  ( 0.8916010070293584056, -0.4528218681382712996, 0.000000000000000000 ) ) ;
#1710 = DIRECTION ( 'NONE',  ( -0.000000000000000000, 1.000000000000000000, -1.387778780781445429E-16 ) ) ;
#1711 = DIRECTION ( 'NONE',  ( -1.000000000000000000, 0.000000000000000000, 0.000000000000000000 ) ) ;
#1712 = TOROIDAL_SURFACE ( 'NONE', #9993, 21.49999999999998224, 1.000000000000000000 ) ;
#1713 = CARTESIAN_POINT ( 'NONE',  ( 187.4999999999996305, 133.0668745871126930, 30.86484227207697018 ) ) ;
#1714 = AXIS2_PLACEMENT_3D ( 'NONE', #13179, #26225, #17323 ) ;
#1715 = CARTESIAN_POINT ( 'NONE',  ( -210.0000000000000568, -157.0000000000000284, 95.00000000000004263 ) ) ;
#1716 = DIRECTION ( 'NONE',  ( 0.000000000000000000, 0.000000000000000000, 1.000000000000000000 ) ) ;
#1717 = DIRECTION ( 'NONE',  ( -1.000000000000000000, -0.000000000000000000, -0.000000000000000000 ) ) ;
#1718 = CARTESIAN_POINT ( 'NONE',  ( 134.9999999999998579, 220.0000000000000284, -99.00000000000001421 ) ) ;
#1719 = ORIENTED_EDGE ( 'NONE', *, *, #1339, .T. ) ;
#1720 = CARTESIAN_POINT ( 'NONE',  ( -201.6083822205884815, 94.40621216759335255, 29.51015678107877349 ) ) ;
#1721 = EDGE_CURVE ( 'NONE', #21449, #20037, #4217, .T. ) ;
#1722 = EDGE_CURVE ( 'NONE', #9931, #11276, #6796, .T. ) ;
#1723 = LINE ( 'NONE', #23710, #21354 ) ;
#1724 = EDGE_LOOP ( 'NONE', ( #4109, #22118, #13477, #16625 ) ) ;
#1725 = VERTEX_POINT ( 'NONE', #15440 ) ;
#1726 = ORIENTED_EDGE ( 'NONE', *, *, #608, .T. ) ;
#1727 = AXIS2_PLACEMENT_3D ( 'NONE', #17796, #18378, #985 ) ;
#1728 = CARTESIAN_POINT ( 'NONE',  ( 118.4313905926795769, 122.3304618272157285, 100.0000000000000142 ) ) ;
#1729 = LINE ( 'NONE', #4316, #20938 ) ;
#1730 = AXIS2_PLACEMENT_3D ( 'NONE', #10382, #16986, #5648 ) ;
#1731 = ORIENTED_EDGE ( 'NONE', *, *, #27128, .T. ) ;
#1732 = EDGE_LOOP ( 'NONE', ( #3173, #18800, #24385, #25189 ) ) ;
#1733 = CARTESIAN_POINT ( 'NONE',  ( 109.5756401952514523, 134.3783162855169451, -89.68749999975639753 ) ) ;
#1734 = FACE_OUTER_BOUND ( 'NONE', #4940, .T. ) ;
#1735 = CARTESIAN_POINT ( 'NONE',  ( -196.6111576902316358, 98.46805465545536151, -31.30665360858167645 ) ) ;
#1736 = VERTEX_POINT ( 'NONE', #1916 ) ;
#1737 = CARTESIAN_POINT ( 'NONE',  ( -233.2943309833551382, 92.06151970357234404, 15.00000000000000000 ) ) ;
#1738 = EDGE_LOOP ( 'NONE', ( #12101, #20635, #18877, #24759 ) ) ;
#1739 = CARTESIAN_POINT ( 'NONE',  ( 232.4749999999995964, 83.06687458711267880, 36.86484227207694175 ) ) ;
#1740 = VECTOR ( 'NONE', #966, 1000.000000000000000 ) ;
#1741 = CARTESIAN_POINT ( 'NONE',  ( 158.0000000000010232, 106.1456246621830957, -45.00000000000000000 ) ) ;
#1742 = CYLINDRICAL_SURFACE ( 'NONE', #24674, 5.000000000000004441 ) ;
#1743 = CARTESIAN_POINT ( 'NONE',  ( -260.0000000000001137, -152.0000000000000284, 105.0000000000000142 ) ) ;
#1744 = VECTOR ( 'NONE', #26376, 1000.000000000000000 ) ;
#1745 = ADVANCED_FACE ( 'NONE', ( #25909 ), #8958, .T. ) ;
#1746 = ORIENTED_EDGE ( 'NONE', *, *, #15857, .T. ) ;
#1747 = CARTESIAN_POINT ( 'NONE',  ( 157.4999999999998579, 78.30506207585207790, 45.00000000000000000 ) ) ;
#1748 = CIRCLE ( 'NONE', #20114, 10.00000000000000888 ) ;
#1749 = CARTESIAN_POINT ( 'NONE',  ( 157.4999999999998295, 228.7775625262745223, -45.00000000000000000 ) ) ;
#1750 = CARTESIAN_POINT ( 'NONE',  ( 109.9999999999999574, -120.0000000000000568, -25.00000000000000711 ) ) ;
#1751 = CARTESIAN_POINT ( 'NONE',  ( -175.0000000000000000, -120.0000000000001705, 64.00000000000002842 ) ) ;
#1752 = VERTEX_POINT ( 'NONE', #17155 ) ;
#1753 = CARTESIAN_POINT ( 'NONE',  ( 119.1248245724174524, 235.9877291319237429, 100.0000000000000142 ) ) ;
#1754 = EDGE_CURVE ( 'NONE', #18948, #27470, #15575, .T. ) ;
#1755 = DIRECTION ( 'NONE',  ( 0.8916010070294395629, -0.4528218681381114274, 0.000000000000000000 ) ) ;
#1756 = CARTESIAN_POINT ( 'NONE',  ( -203.1779787704217313, 93.05164332230201296, 28.77272332722132120 ) ) ;
#1757 = ORIENTED_EDGE ( 'NONE', *, *, #20832, .T. ) ;
#1758 = SHAPE_REPRESENTATION_RELATIONSHIP ( 'NONE' , 'NONE' ,  #18912, #11228 ) ;
#1759 = FACE_OUTER_BOUND ( 'NONE', #21101, .T. ) ;
#1760 = ORIENTED_EDGE ( 'NONE', *, *, #5776, .F. ) ;
#1761 = EDGE_CURVE ( 'NONE', #21329, #13313, #21888, .T. ) ;
#1762 = DIRECTION ( 'NONE',  ( -1.321694076934710155E-16, 1.000000000000000000, 0.000000000000000000 ) ) ;
#1763 = VECTOR ( 'NONE', #14890, 1000.000000000000000 ) ;
#1764 = CARTESIAN_POINT ( 'NONE',  ( -173.2914958970121404, 113.9438874222513789, -27.61821649288708969 ) ) ;
#1765 = EDGE_LOOP ( 'NONE', ( #4521, #6128, #4628, #3710 ) ) ;
#1766 = ORIENTED_EDGE ( 'NONE', *, *, #18746, .T. ) ;
#1767 = DIRECTION ( 'NONE',  ( 0.000000000000000000, 0.000000000000000000, -1.000000000000000000 ) ) ;
#1768 = ORIENTED_EDGE ( 'NONE', *, *, #2402, .T. ) ;
#1769 = VECTOR ( 'NONE', #4087, 1000.000000000000000 ) ;
#1770 = VECTOR ( 'NONE', #27706, 1000.000000000000000 ) ;
#1771 = ORIENTED_EDGE ( 'NONE', *, *, #23602, .T. ) ;
#1772 = EDGE_LOOP ( 'NONE', ( #25202, #14510, #24999, #3530, #23753 ) ) ;
#1773 = EDGE_CURVE ( 'NONE', #3789, #4186, #11736, .T. ) ;
#1774 = DIRECTION ( 'NONE',  ( 1.000000000000000000, 0.000000000000000000, 0.000000000000000000 ) ) ;
#1775 = CARTESIAN_POINT ( 'NONE',  ( 232.4999999999996305, 83.06687458711267880, 30.86484227207694886 ) ) ;
#1776 = PLANE ( 'NONE',  #8728 ) ;
#1777 = DIRECTION ( 'NONE',  ( 0.000000000000000000, 0.000000000000000000, -1.000000000000000000 ) ) ;
#1778 = CARTESIAN_POINT ( 'NONE',  ( 157.4999999999997726, 246.3326875788235384, -45.00000000000000000 ) ) ;
#1779 = EDGE_CURVE ( 'NONE', #9971, #24116, #6235, .T. ) ;
#1780 = CARTESIAN_POINT ( 'NONE',  ( -231.9024517383451212, 76.40908368390745409, -15.65418338381065944 ) ) ;
#1781 = ORIENTED_EDGE ( 'NONE', *, *, #17710, .F. ) ;
#1782 = VECTOR ( 'NONE', #5929, 1000.000000000000000 ) ;
#1783 = LINE ( 'NONE', #3806, #16806 ) ;
#1784 = CIRCLE ( 'NONE', #24289, 6.000000000000005329 ) ;
#1785 = CARTESIAN_POINT ( 'NONE',  ( -217.2892621185082760, 109.4029876883478352, -15.00000000000000000 ) ) ;
#1786 = CARTESIAN_POINT ( 'NONE',  ( 157.4999999999998579, 196.1751874286831026, 45.00000000000000000 ) ) ;
#1787 = DIRECTION ( 'NONE',  ( -0.8916010070293383105, -0.4528218681383106015, 0.000000000000000000 ) ) ;
#1788 = VERTEX_POINT ( 'NONE', #2478 ) ;
#1789 = CARTESIAN_POINT ( 'NONE',  ( 0.3651377029009472142, 1.249999999999999556, -7.402212548643259282 ) ) ;
#1790 = AXIS2_PLACEMENT_3D ( 'NONE', #5010, #4866, #7323 ) ;
#1791 = LINE ( 'NONE', #13023, #4249 ) ;
#1792 = CARTESIAN_POINT ( 'NONE',  ( -262.5215738956072755, -166.3598102777078509, 89.99999999999998579 ) ) ;
#1793 = PLANE ( 'NONE',  #9859 ) ;
#1794 = CARTESIAN_POINT ( 'NONE',  ( 222.4999999999996021, 186.4134324495536248, 35.02193266779035952 ) ) ;
#1795 = VERTEX_POINT ( 'NONE', #17718 ) ;
#1796 = VECTOR ( 'NONE', #3292, 1000.000000000000000 ) ;
#1797 = EDGE_CURVE ( 'NONE', #18321, #16168, #19453, .T. ) ;
#1798 = LINE ( 'NONE', #17313, #12537 ) ;
#1799 = VERTEX_POINT ( 'NONE', #22029 ) ;
#1800 = EDGE_CURVE ( 'NONE', #14705, #25689, #6207, .T. ) ;
#1801 = CARTESIAN_POINT ( 'NONE',  ( 157.9999999999997726, 243.5708750675630370, 45.00000000000000000 ) ) ;
#1802 = ORIENTED_EDGE ( 'NONE', *, *, #22126, .T. ) ;
#1803 = ORIENTED_EDGE ( 'NONE', *, *, #23982, .T. ) ;
#1804 = CARTESIAN_POINT ( 'NONE',  ( -140.1213116003368668, 122.5384136796733827, -15.00000000000000000 ) ) ;
#1805 = VECTOR ( 'NONE', #9490, 1000.000000000000114 ) ;
#1806 = VECTOR ( 'NONE', #25098, 1000.000000000000000 ) ;
#1807 = ORIENTED_EDGE ( 'NONE', *, *, #20147, .F. ) ;
#1808 = VERTEX_POINT ( 'NONE', #19593 ) ;
#1809 = CARTESIAN_POINT ( 'NONE',  ( 0.000000000000000000, 0.000000000000000000, 100.0000000000000000 ) ) ;
#1810 = ADVANCED_FACE ( 'NONE', ( #6661 ), #11116, .T. ) ;
#1811 = CARTESIAN_POINT ( 'NONE',  ( -97.59841077035456181, 134.4761401613473879, -15.51281503506764814 ) ) ;
#1812 = PLANE ( 'NONE',  #12527 ) ;
#1813 = VECTOR ( 'NONE', #24340, 1000.000000000000114 ) ;
#1814 = EDGE_CURVE ( 'NONE', #1940, #20107, #4489, .T. ) ;
#1815 = CARTESIAN_POINT ( 'NONE',  ( -142.1390311221107368, 127.5729955578239156, -17.65724288274918763 ) ) ;
#1816 = AXIS2_PLACEMENT_3D ( 'NONE', #8716, #6696, #21924 ) ;
#1817 = CARTESIAN_POINT ( 'NONE',  ( -267.0129679999498649, -170.7675089197775264, -89.18277029719632765 ) ) ;
#1818 = CARTESIAN_POINT ( 'NONE',  ( -266.3037744482016365, -165.6613878827935196, 89.35851331749265114 ) ) ;
#1819 = CARTESIAN_POINT ( 'NONE',  ( -211.3790541256307733, 87.57060272315374050, -24.25130854840332617 ) ) ;
#1820 = CARTESIAN_POINT ( 'NONE',  ( 128.9998022404941480, 249.3938365459133593, -145.3931298709317446 ) ) ;
#1821 = CARTESIAN_POINT ( 'NONE',  ( -262.5802634612744555, -171.5969890882419406, -94.99999999999990052 ) ) ;
#1822 = EDGE_CURVE ( 'NONE', #24930, #20966, #20446, .T. ) ;
#1823 = DIRECTION ( 'NONE',  ( -0.8916010070293584056, 0.4528218681382713551, 0.000000000000000000 ) ) ;
#1824 = CARTESIAN_POINT ( 'NONE',  ( -160.0000000000000284, 59.99999999999994316, -15.00000000000000000 ) ) ;
#1825 = DIRECTION ( 'NONE',  ( 0.8916010070293584056, -0.4528218681382712996, 0.000000000000000000 ) ) ;
#1826 = ORIENTED_EDGE ( 'NONE', *, *, #5486, .F. ) ;
#1827 = VECTOR ( 'NONE', #25631, 1000.000000000000000 ) ;
#1828 = CARTESIAN_POINT ( 'NONE',  ( 158.0000000000011937, 93.09837461714084839, -45.00000000000000000 ) ) ;
#1829 = DIRECTION ( 'NONE',  ( -0.8916010070296936929, -0.4528218681376112165, 0.000000000000000000 ) ) ;
#1830 = CARTESIAN_POINT ( 'NONE',  ( 157.9999999999996874, 266.6496251426330559, 45.00000000000000000 ) ) ;
#1832 = ORIENTED_EDGE ( 'NONE', *, *, #12580, .T. ) ;
#1831 = ORIENTED_EDGE ( 'NONE', *, *, #2595, .F. ) ;
#1833 = VECTOR ( 'NONE', #27757, 1000.000000000000000 ) ;
#1834 = CARTESIAN_POINT ( 'NONE',  ( 103.7569845406462861, 245.1294976011695894, -26.47883977339530759 ) ) ;
#1835 = ORIENTED_EDGE ( 'NONE', *, *, #7098, .T. ) ;
#1836 = ORIENTED_EDGE ( 'NONE', *, *, #4245, .T. ) ;
#1837 = ORIENTED_EDGE ( 'NONE', *, *, #8083, .F. ) ;
#1838 = ORIENTED_EDGE ( 'NONE', *, *, #24573, .T. ) ;
#1839 = EDGE_LOOP ( 'NONE', ( #24486, #23427, #15466, #10507 ) ) ;
#1840 = ORIENTED_EDGE ( 'NONE', *, *, #2826, .T. ) ;
#1841 = DIRECTION ( 'NONE',  ( 0.000000000000000000, -1.000000000000000000, 0.000000000000000000 ) ) ;
#1842 = AXIS2_PLACEMENT_3D ( 'NONE', #7567, #9854, #18200 ) ;
#1843 = DIRECTION ( 'NONE',  ( 0.000000000000000000, 0.000000000000000000, -1.000000000000000000 ) ) ;
#1844 = ADVANCED_FACE ( 'NONE', ( #4356 ), #17291, .F. ) ;
#1845 = DIRECTION ( 'NONE',  ( 0.4528218681377511601, 0.8916010070296226386, -0.000000000000000000 ) ) ;
#1846 = ADVANCED_FACE ( 'NONE', ( #17434 ), #21604, .T. ) ;
#1847 = AXIS2_PLACEMENT_3D ( 'NONE', #23597, #26024, #27887 ) ;
#1848 = LINE ( 'NONE', #17364, #5052 ) ;
#1849 = CARTESIAN_POINT ( 'NONE',  ( -271.2644327268766915, -165.3329768350718041, -108.7419004184296369 ) ) ;
#1850 = CARTESIAN_POINT ( 'NONE',  ( 158.0000000000003411, 175.8582498648732440, 45.00000000000000000 ) ) ;
#1851 = DIRECTION ( 'NONE',  ( -0.000000000000000000, 1.000000000000000000, -1.387778780781445429E-16 ) ) ;
#1852 = CARTESIAN_POINT ( 'NONE',  ( -31.50759449548381497, 129.2243747201668214, 15.65997819548621628 ) ) ;
#1853 = B_SPLINE_CURVE_WITH_KNOTS ( 'NONE', 3,
 ( #989, #3273, #3419, #18524, #719, #24846, #7468, #9765, #853, #14083, #12213, #20814, #11927, #20952, #14499, #22833, #3558, #16097, #27268, #5722, #20528, #7609 ),
 .UNSPECIFIED., .F., .F.,
 ( 4, 2, 2, 2, 2, 2, 2, 2, 2, 2, 4 ),
 ( 0.000000000000000000, 0.1249999999999999306, 0.2500000000000000555, 0.3750000000000000000, 0.5000000000000000000, 0.6250000000000000000, 0.7500000000000000000, 0.8125000000000000000, 0.8750000000000001110, 0.9374999999999998890, 1.000000000000000000 ),
 .UNSPECIFIED. ) ;
#1854 = DIRECTION ( 'NONE',  ( 0.000000000000000000, 0.000000000000000000, 1.000000000000000000 ) ) ;
#1855 = DIRECTION ( 'NONE',  ( 0.000000000000000000, -1.387778780781445429E-16, -1.000000000000000000 ) ) ;
#1856 = CARTESIAN_POINT ( 'NONE',  ( 65.00000000000000000, -150.0000000000000568, 76.00000000000001421 ) ) ;
#1857 = ORIENTED_EDGE ( 'NONE', *, *, #15799, .T. ) ;
#1858 = CARTESIAN_POINT ( 'NONE',  ( 119.9999999999998863, 330.0000000000000000, 90.00000000000002842 ) ) ;
#1859 = AXIS2_PLACEMENT_3D ( 'NONE', #1470, #21003, #18999 ) ;
#1860 = DIRECTION ( 'NONE',  ( -0.8916010070293783896, 0.4528218681382319422, 0.000000000000000000 ) ) ;
#1861 = ORIENTED_EDGE ( 'NONE', *, *, #10332, .T. ) ;
#1862 = APPLICATION_PROTOCOL_DEFINITION ( 'draft international standard', 'automotive_design', 1998, #2664 ) ;
#1863 = ORIENTED_EDGE ( 'NONE', *, *, #6822, .T. ) ;
#1864 = ORIENTED_EDGE ( 'NONE', *, *, #11211, .F. ) ;
#1865 = CIRCLE ( 'NONE', #25736, 7.685040811306672381 ) ;
#1866 = CARTESIAN_POINT ( 'NONE',  ( 81.45493510947169113, 110.0000000031298981, 100.0000000000000142 ) ) ;
#1867 = EDGE_CURVE ( 'NONE', #20330, #25368, #19872, .T. ) ;
#1868 = LINE ( 'NONE', #10646, #5333 ) ;
#1869 = ORIENTED_EDGE ( 'NONE', *, *, #5831, .T. ) ;
#1870 = ORIENTED_EDGE ( 'NONE', *, *, #3281, .F. ) ;
#1871 = CARTESIAN_POINT ( 'NONE',  ( 96.76194576697405125, 83.89264379418708018, -100.0000000000000284 ) ) ;
#1872 = DIRECTION ( 'NONE',  ( 0.000000000000000000, -0.9458112779747414045, 0.3247168404252948615 ) ) ;
#1873 = FACE_OUTER_BOUND ( 'NONE', #25346, .T. ) ;
#1874 = VERTEX_POINT ( 'NONE', #13418 ) ;
#1875 = ADVANCED_FACE ( 'NONE', ( #345 ), #14134, .F. ) ;
#1876 = CARTESIAN_POINT ( 'NONE',  ( -227.8046702420875533, 90.53362311475710555, 13.46331733193806102 ) ) ;
#1877 = VERTEX_POINT ( 'NONE', #15723 ) ;
#1878 = CARTESIAN_POINT ( 'NONE',  ( -46.68942599940377391, -18.01420295945611727, 100.0000000000000000 ) ) ;
#1879 = EDGE_CURVE ( 'NONE', #16598, #25488, #13714, .T. ) ;
#1880 = EDGE_CURVE ( 'NONE', #16325, #26049, #22463, .T. ) ;
#1881 = VECTOR ( 'NONE', #15054, 1000.000000000000000 ) ;
#1882 = EDGE_CURVE ( 'NONE', #21087, #5617, #8959, .T. ) ;
#1883 = DIRECTION ( 'NONE',  ( -0.8916010070299268397, 0.4528218681371523058, 0.000000000000000000 ) ) ;
#1884 = CARTESIAN_POINT ( 'NONE',  ( 158.0554390835131642, 200.8047184523794897, -141.8266621613457232 ) ) ;
#1885 = AXIS2_PLACEMENT_3D ( 'NONE', #20179, #11860, #26790 ) ;
#1886 = CARTESIAN_POINT ( 'NONE',  ( 157.4999999999996589, 281.4429376839215138, -45.00000000000000000 ) ) ;
#1887 = VECTOR ( 'NONE', #26855, 1000.000000000000114 ) ;
#1888 = EDGE_LOOP ( 'NONE', ( #7302, #12887 ) ) ;
#1889 = DIRECTION ( 'NONE',  ( 1.000000000000000000, 0.000000000000000000, -0.000000000000000000 ) ) ;
#1890 = LINE ( 'NONE', #24028, #11986 ) ;
#1891 = LINE ( 'NONE', #10668, #22112 ) ;
#1892 = DIRECTION ( 'NONE',  ( 0.5457381880580697286, -0.8379557447115539848, 0.000000000000000000 ) ) ;
#1893 = ORIENTED_EDGE ( 'NONE', *, *, #17759, .T. ) ;
#1894 = LINE ( 'NONE', #19851, #17393 ) ;
#1895 = FACE_OUTER_BOUND ( 'NONE', #25198, .T. ) ;
#1896 = CARTESIAN_POINT ( 'NONE',  ( -17.24491960465745777, -18.01420295945611727, 95.00000000000000000 ) ) ;
#1897 = DIRECTION ( 'NONE',  ( 1.000000000000000000, 0.000000000000000000, 0.000000000000000000 ) ) ;
#1898 = ORIENTED_EDGE ( 'NONE', *, *, #11888, .T. ) ;
#1899 = SHAPE_REPRESENTATION_RELATIONSHIP ( 'NONE' , 'NONE' ,  #201, #25288 ) ;
#1900 = DIRECTION ( 'NONE',  ( -0.000000000000000000, -0.000000000000000000, -1.000000000000000000 ) ) ;
#1901 = ORIENTED_EDGE ( 'NONE', *, *, #16079, .T. ) ;
#1902 = AXIS2_PLACEMENT_3D ( 'NONE', #7946, #10109, #6209 ) ;
#1903 = DIRECTION ( 'NONE',  ( 0.000000000000000000, 0.000000000000000000, 1.000000000000000000 ) ) ;
#1904 = CARTESIAN_POINT ( 'NONE',  ( -188.5440957081713407, 104.2034936733272161, -32.76882375805663372 ) ) ;
#1905 = VERTEX_POINT ( 'NONE', #22318 ) ;
#1906 = VECTOR ( 'NONE', #23751, 1000.000000000000000 ) ;
#1907 = AXIS2_PLACEMENT_3D ( 'NONE', #13162, #26068, #19181 ) ;
#1908 = VERTEX_POINT ( 'NONE', #16150 ) ;
#1909 = CARTESIAN_POINT ( 'NONE',  ( -110.7275636018716654, 68.51688903468615877, 83.00000000000001421 ) ) ;
#1910 = ORIENTED_EDGE ( 'NONE', *, *, #5300, .F. ) ;
#1911 = EDGE_CURVE ( 'NONE', #10196, #24950, #3053, .T. ) ;
#1912 = ORIENTED_EDGE ( 'NONE', *, *, #259, .F. ) ;
#1913 = VERTEX_POINT ( 'NONE', #17861 ) ;
#1914 = FACE_OUTER_BOUND ( 'NONE', #10500, .T. ) ;
#1915 = ADVANCED_FACE ( 'NONE', ( #908 ), #24473, .F. ) ;
#1916 = CARTESIAN_POINT ( 'NONE',  ( 119.1329331941753225, 207.8247714198252254, -45.00000000000000000 ) ) ;
#1917 = LINE ( 'NONE', #10698, #3383 ) ;
#1918 = CARTESIAN_POINT ( 'NONE',  ( 67.86343429515802939, -22.14858123305036486, -45.00000000000000000 ) ) ;
#1919 = CARTESIAN_POINT ( 'NONE',  ( -207.7359966080777554, 74.87654876227064449, -43.86827885981523423 ) ) ;
#1920 = CARTESIAN_POINT ( 'NONE',  ( -79.00187704905530950, 96.44595867864546790, -145.0000000000000000 ) ) ;
#1921 = CARTESIAN_POINT ( 'NONE',  ( -226.6109647993037868, 62.69877383611189003, -18.44381613004360432 ) ) ;
#1922 = ORIENTED_EDGE ( 'NONE', *, *, #27086, .T. ) ;
#1923 = VECTOR ( 'NONE', #18549, 999.9999999999998863 ) ;
#1924 = FACE_OUTER_BOUND ( 'NONE', #19298, .T. ) ;
#1925 = CARTESIAN_POINT ( 'NONE',  ( 157.4999999999998579, 123.4468122109788482, 45.00000000000000000 ) ) ;
#1927 = DIRECTION ( 'NONE',  ( -0.000000000000000000, -1.000000000000000000, -0.000000000000000000 ) ) ;
#1926 = VECTOR ( 'NONE', #10361, 1000.000000000000000 ) ;
#1928 = CARTESIAN_POINT ( 'NONE',  ( 157.9999999999999147, 213.9842499849850697, -45.00000000000000000 ) ) ;
#1929 = PRODUCT_DEFINITION_FORMATION_WITH_SPECIFIED_SOURCE ( 'ANY', '', #18972, .NOT_KNOWN. ) ;
#1930 = ORIENTED_EDGE ( 'NONE', *, *, #21678, .T. ) ;
#1931 = CARTESIAN_POINT ( 'NONE',  ( -86.45101491668415861, -42.20485572845630884, -15.00000000000000000 ) ) ;
#1932 = CIRCLE ( 'NONE', #12073, 6.025000000000002132 ) ;
#1933 = CARTESIAN_POINT ( 'NONE',  ( 157.4999999999998579, 65.76568703831686946, 45.00000000000000000 ) ) ;
#1934 = CARTESIAN_POINT ( 'NONE',  ( 158.0000000000002558, 183.3818748873943889, -45.00000000000000000 ) ) ;
#1935 = CARTESIAN_POINT ( 'NONE',  ( 157.4999999999998010, 241.3169375638095460, 45.00000000000000000 ) ) ;
#1936 = LINE ( 'NONE', #8836, #19345 ) ;
#1937 = DIRECTION ( 'NONE',  ( 0.000000000000000000, 0.000000000000000000, -1.000000000000000000 ) ) ;
#1938 = ORIENTED_EDGE ( 'NONE', *, *, #7675, .F. ) ;
#1939 = DIRECTION ( 'NONE',  ( 0.000000000000000000, 0.000000000000000000, -1.000000000000000000 ) ) ;
#1940 = VERTEX_POINT ( 'NONE', #771 ) ;
#1941 = CARTESIAN_POINT ( 'NONE',  ( 112.4999999999998863, 220.0000000000000284, -90.00000000000002842 ) ) ;
#1942 = ORIENTED_EDGE ( 'NONE', *, *, #3569, .F. ) ;
#1943 = VERTEX_POINT ( 'NONE', #4921 ) ;
#1944 = CARTESIAN_POINT ( 'NONE',  ( 112.4999999999998863, 220.0000000000000284, 90.00000000000002842 ) ) ;
#1945 = EDGE_LOOP ( 'NONE', ( #6961, #13309, #1870, #11630 ) ) ;
#1946 = EDGE_CURVE ( 'NONE', #15640, #16689, #12202, .T. ) ;
#1947 = CIRCLE ( 'NONE', #20308, 5.000000000000004441 ) ;
#1948 = EDGE_LOOP ( 'NONE', ( #12224, #23472, #16271, #17867 ) ) ;
#1949 = ORIENTED_EDGE ( 'NONE', *, *, #2985, .F. ) ;
#1950 = VECTOR ( 'NONE', #12093, 1000.000000000000227 ) ;
#1951 = DIRECTION ( 'NONE',  ( 0.000000000000000000, 0.000000000000000000, 1.000000000000000000 ) ) ;
#1952 = LINE ( 'NONE', #12471, #4085 ) ;
#1953 = DIRECTION ( 'NONE',  ( -0.8916010070296124246, 0.4528218681377710886, 0.000000000000000000 ) ) ;
#1954 = VECTOR ( 'NONE', #23788, 999.9999999999998863 ) ;
#1955 = DIRECTION ( 'NONE',  ( -0.5000000000000039968, -0.8660254037844362651, -1.224646799147353454E-16 ) ) ;
#1956 = DIRECTION ( 'NONE',  ( -0.000000000000000000, 0.000000000000000000, -1.000000000000000000 ) ) ;
#1957 = CARTESIAN_POINT ( 'NONE',  ( -266.0153270024459289, -170.9359483083451039, -94.62226971369513251 ) ) ;
#1958 = CARTESIAN_POINT ( 'NONE',  ( -270.3796563303090466, -170.3242331377992684, 88.15587544550923838 ) ) ;
#1959 = CARTESIAN_POINT ( 'NONE',  ( -231.4227546898554522, 93.05579960084709512, -15.01574783250532974 ) ) ;
#1960 = EDGE_CURVE ( 'NONE', #19398, #28117, #22608, .T. ) ;
#1961 = EDGE_CURVE ( 'NONE', #7303, #3747, #16290, .T. ) ;
#1962 = CARTESIAN_POINT ( 'NONE',  ( 133.0594107791237661, 249.9377649212624419, -150.6809294437986182 ) ) ;
#1963 = DIRECTION ( 'NONE',  ( -0.8916010070299875689, 0.4528218681370324017, 0.000000000000000000 ) ) ;
#1964 = CARTESIAN_POINT ( 'NONE',  ( -277.2150368962633706, -237.2150368962634559, -109.9999999999998153 ) ) ;
#1965 = PLANE ( 'NONE',  #18741 ) ;
#1966 = DIRECTION ( 'NONE',  ( 1.000000000000000000, 0.000000000000000000, 0.000000000000000000 ) ) ;
#1967 = ORIENTED_EDGE ( 'NONE', *, *, #9632, .T. ) ;
#1968 = VECTOR ( 'NONE', #7525, 1000.000000000000000 ) ;
#1969 = AXIS2_PLACEMENT_3D ( 'NONE', #5932, #12840, #14856 ) ;
#1970 = CARTESIAN_POINT ( 'NONE',  ( 158.0000000000009663, 113.1613746771971876, 45.00000000000000000 ) ) ;
#1971 = DIRECTION ( 'NONE',  ( 0.000000000000000000, 0.000000000000000000, 1.000000000000000000 ) ) ;
#1972 = CARTESIAN_POINT ( 'NONE',  ( 107.7878109108858098, 207.3655475159964681, -150.3903514073973611 ) ) ;
#1973 = VECTOR ( 'NONE', #25367, 1000.000000000000000 ) ;
#1974 = EDGE_LOOP ( 'NONE', ( #18192, #8711 ) ) ;
#1975 = EDGE_CURVE ( 'NONE', #3327, #9386, #24902, .T. ) ;
#1976 = AXIS2_PLACEMENT_3D ( 'NONE', #3956, #4099, #27934 ) ;
#1977 = EDGE_CURVE ( 'NONE', #23487, #10355, #2919, .T. ) ;
#1978 = CARTESIAN_POINT ( 'NONE',  ( 94.04374108504291030, 240.3974664687522420, -8.346404539541740775 ) ) ;
#1979 = ORIENTED_EDGE ( 'NONE', *, *, #26840, .T. ) ;
#1980 = DIRECTION ( 'NONE',  ( 1.000000000000000000, -0.000000000000000000, -0.000000000000000000 ) ) ;
#1981 = VERTEX_POINT ( 'NONE', #9398 ) ;
#1982 = VERTEX_POINT ( 'NONE', #20445 ) ;
#1983 = ORIENTED_EDGE ( 'NONE', *, *, #10135, .F. ) ;
#1984 = ORIENTED_EDGE ( 'NONE', *, *, #18001, .T. ) ;
#1985 = ORIENTED_EDGE ( 'NONE', *, *, #28042, .T. ) ;
#1986 = VECTOR ( 'NONE', #24400, 1000.000000000000000 ) ;
#1987 = CARTESIAN_POINT ( 'NONE',  ( 158.0000000000001705, 190.9054999099155054, 45.00000000000000000 ) ) ;
#1988 = VECTOR ( 'NONE', #19866, 1000.000000000000000 ) ;
#1989 = DIRECTION ( 'NONE',  ( 0.8916010070293383105, -0.4528218681383106015, 0.000000000000000000 ) ) ;
#1990 = VECTOR ( 'NONE', #24485, 1000.000000000000000 ) ;
#1991 = PRODUCT_DEFINITION_CONTEXT ( 'detailed design', #14803, 'design' ) ;
#1992 = DIRECTION ( 'NONE',  ( 1.000000000000000000, -0.000000000000000000, -0.000000000000000000 ) ) ;
#1993 = ADVANCED_FACE ( 'NONE', ( #20301 ), #18155, .F. ) ;
#1994 = LINE ( 'NONE', #4004, #23887 ) ;
#1995 = LINE ( 'NONE', #1326, #26382 ) ;
#1996 = EDGE_CURVE ( 'NONE', #19047, #23530, #18298, .T. ) ;
#1997 = LINE ( 'NONE', #4574, #7104 ) ;
#1998 = LINE ( 'NONE', #8899, #22392 ) ;
#1999 = DIRECTION ( 'NONE',  ( 1.000000000000000000, 0.000000000000000000, -0.000000000000000000 ) ) ;
#2000 = CARTESIAN_POINT ( 'NONE',  ( -23.49204859636672893, 128.1179884427479294, 17.45313152111423705 ) ) ;
#2001 = DIRECTION ( 'NONE',  ( 1.000000000000000000, 0.000000000000000000, 0.000000000000000000 ) ) ;
#2002 = CARTESIAN_POINT ( 'NONE',  ( -210.0000000000000568, -220.0000000000000853, 110.0000000000000284 ) ) ;
#2003 = DIRECTION ( 'NONE',  ( -4.540956701092242152E-16, -1.000000000000000000, -0.000000000000000000 ) ) ;
#2005 = VERTEX_POINT ( 'NONE', #9677 ) ;
#2004 = ORIENTED_EDGE ( 'NONE', *, *, #27343, .T. ) ;
#2006 = VECTOR ( 'NONE', #26913, 1000.000000000000227 ) ;
#2007 = CARTESIAN_POINT ( 'NONE',  ( -173.0260071355321543, 113.6300340977356029, 28.16161390424484878 ) ) ;
#2008 = DIRECTION ( 'NONE',  ( 1.000000000000000000, 0.000000000000000000, 0.000000000000000000 ) ) ;
#2009 = VERTEX_POINT ( 'NONE', #7382 ) ;
#2010 = CONTEXT_DEPENDENT_SHAPE_REPRESENTATION ( #668, #25621 ) ;
#2011 = VECTOR ( 'NONE', #1337, 1000.000000000000000 ) ;
#2012 = VERTEX_POINT ( 'NONE', #18437 ) ;
#2013 = EDGE_CURVE ( 'NONE', #23466, #21067, #4383, .T. ) ;
#2015 = EDGE_CURVE ( 'NONE', #21206, #27854, #20721, .T. ) ;
#2014 = ORIENTED_EDGE ( 'NONE', *, *, #1373, .T. ) ;
#2016 = CARTESIAN_POINT ( 'NONE',  ( 134.9999999999998579, 220.0000000000000284, -84.99999999999997158 ) ) ;
#2017 = PLANE ( 'NONE',  #8080 ) ;
#2018 = VERTEX_POINT ( 'NONE', #18010 ) ;
#2019 = EDGE_CURVE ( 'NONE', #17098, #12396, #27748, .T. ) ;
#2020 = EDGE_LOOP ( 'NONE', ( #722, #7286, #1075, #6184, #18708, #10466 ) ) ;
#2021 = CARTESIAN_POINT ( 'NONE',  ( 98.15430812627619162, 116.0637945822588364, -100.0000000000433005 ) ) ;
#2022 = LINE ( 'NONE', #10798, #27634 ) ;
#2023 = VECTOR ( 'NONE', #1142, 1000.000000000000000 ) ;
#2024 = CARTESIAN_POINT ( 'NONE',  ( -169.9623962693859482, 115.7491617292054826, -25.38483726571820753 ) ) ;
#2025 = ORIENTED_EDGE ( 'NONE', *, *, #1880, .T. ) ;
#2026 = CARTESIAN_POINT ( 'NONE',  ( -224.4716126166392485, 89.01384884033475942, 16.47823558538952682 ) ) ;
#2027 = EDGE_LOOP ( 'NONE', ( #9558, #1359, #12496, #26792 ) ) ;
#2028 = CONICAL_SURFACE ( 'NONE', #13511, 5.999999999999977796, 1.029744258676652979 ) ;
#2029 = DIRECTION ( 'NONE',  ( 0.000000000000000000, -1.000000000000000000, 0.000000000000000000 ) ) ;
#2030 = CARTESIAN_POINT ( 'NONE',  ( -146.6428522700808230, 69.54464929955099706, 80.00000000000001421 ) ) ;
#2031 = VECTOR ( 'NONE', #4410, 1000.000000000000000 ) ;
#2032 = CARTESIAN_POINT ( 'NONE',  ( 160.5791959497488222, 204.3237910346065291, -139.0484678162420380 ) ) ;
#2033 = CARTESIAN_POINT ( 'NONE',  ( 232.4999999999996305, 133.0668745871126930, 36.86484227207694886 ) ) ;
#2034 = ORIENTED_EDGE ( 'NONE', *, *, #19694, .T. ) ;
#2035 = CARTESIAN_POINT ( 'NONE',  ( 115.9304285313496905, 208.0449276593521688, 99.14012769162644645 ) ) ;
#2036 = FACE_OUTER_BOUND ( 'NONE', #4668, .T. ) ;
#2037 = PLANE ( 'NONE',  #3279 ) ;
#2038 = DIRECTION ( 'NONE',  ( 0.000000000000000000, 0.000000000000000000, 1.000000000000000000 ) ) ;
#2039 = ORIENTED_EDGE ( 'NONE', *, *, #19310, .F. ) ;
#2040 = CARTESIAN_POINT ( 'NONE',  ( 9.345921402568901470, 140.0000000000000000, 15.00000000000000000 ) ) ;
#2041 = DIRECTION ( 'NONE',  ( 0.000000000000000000, 1.000000000000000000, 0.000000000000000000 ) ) ;
#2042 = DIRECTION ( 'NONE',  ( -1.000000000000000000, 6.938893903907227392E-16, 0.000000000000000000 ) ) ;
#2043 = CARTESIAN_POINT ( 'NONE',  ( -40.40953891503691153, 71.03850157808263077, 100.0000000000000000 ) ) ;
#2044 = EDGE_LOOP ( 'NONE', ( #13113, #23691 ) ) ;
#2045 = EDGE_CURVE ( 'NONE', #27342, #12331, #5777, .T. ) ;
#2046 = ORIENTED_EDGE ( 'NONE', *, *, #15839, .T. ) ;
#2047 = EDGE_CURVE ( 'NONE', #13726, #5026, #18575, .T. ) ;
#2048 = CARTESIAN_POINT ( 'NONE',  ( 157.4999999999998579, 193.6673124211760353, 45.00000000000000000 ) ) ;
#2049 = EDGE_CURVE ( 'NONE', #88, #24530, #1995, .T. ) ;
#2050 = CARTESIAN_POINT ( 'NONE',  ( -185.8938050120760295, 106.2234131628355414, -31.95887621392303046 ) ) ;
#2051 = ORIENTED_EDGE ( 'NONE', *, *, #11624, .T. ) ;
#2052 = VECTOR ( 'NONE', #18137, 1000.000000000000114 ) ;
#2053 = ORIENTED_EDGE ( 'NONE', *, *, #2765, .T. ) ;
#2054 = FACE_OUTER_BOUND ( 'NONE', #7891, .T. ) ;
#2055 = ORIENTED_EDGE ( 'NONE', *, *, #22306, .F. ) ;
#2056 = CARTESIAN_POINT ( 'NONE',  ( -146.6428522700808230, 17.24192588826928585, 83.00000000000001421 ) ) ;
#2057 = ORIENTED_EDGE ( 'NONE', *, *, #18923, .T. ) ;
#2058 = ORIENTED_EDGE ( 'NONE', *, *, #23518, .T. ) ;
#2059 = DIRECTION ( 'NONE',  ( 1.000000000000000000, -0.000000000000000000, -0.000000000000000000 ) ) ;
#2060 = CARTESIAN_POINT ( 'NONE',  ( 93.99999999999985789, 268.4896896257338312, -105.0000000000000284 ) ) ;
#2061 = CARTESIAN_POINT ( 'NONE',  ( 0.000000000000000000, 1.249999999999999556, 6.997769477110050929 ) ) ;
#2062 = FACE_OUTER_BOUND ( 'NONE', #20613, .T. ) ;
#2063 = CIRCLE ( 'NONE', #16327, 5.999999999999991118 ) ;
#2064 = CARTESIAN_POINT ( 'NONE',  ( -262.5514013678064771, -171.6040736444017512, 105.0000000000000000 ) ) ;
#2065 = DIRECTION ( 'NONE',  ( 1.000000000000000000, 0.000000000000000000, 0.000000000000000000 ) ) ;
#2066 = CARTESIAN_POINT ( 'NONE',  ( -229.4479296852199752, 74.49644851801838286, -16.38316105114333965 ) ) ;
#2067 = EDGE_LOOP ( 'NONE', ( #1560, #12873, #23006, #5591 ) ) ;
#2068 = LINE ( 'NONE', #20020, #17266 ) ;
#2069 = CIRCLE ( 'NONE', #264, 10.00000000000000888 ) ;
#2070 = DIRECTION ( 'NONE',  ( 1.000000000000000000, 0.000000000000000000, 0.000000000000000000 ) ) ;
#2071 = CARTESIAN_POINT ( 'NONE',  ( -2.081668171172168513E-14, 79.99999999999998579, -100.0000000000000142 ) ) ;
#2072 = DIRECTION ( 'NONE',  ( 0.000000000000000000, -1.000000000000000000, 0.000000000000000000 ) ) ;
#2073 = ORIENTED_EDGE ( 'NONE', *, *, #6135, .T. ) ;
#2074 = LINE ( 'NONE', #13160, #28386 ) ;
#2075 = ADVANCED_FACE ( 'NONE', ( #9953 ), #7662, .F. ) ;
#2076 = DIRECTION ( 'NONE',  ( -1.000000000000000000, 0.000000000000000000, 0.000000000000000000 ) ) ;
#2077 = DIRECTION ( 'NONE',  ( -0.8916010070293384215, 0.4528218681383106015, 0.000000000000000000 ) ) ;
#2078 = DIRECTION ( 'NONE',  ( 0.8916010070294199119, 0.4528218681381501742, 0.000000000000000000 ) ) ;
#2079 = DIRECTION ( 'NONE',  ( 0.4528218681381700472, -0.8916010070294099199, 0.000000000000000000 ) ) ;
#2080 =( NAMED_UNIT ( * ) PLANE_ANGLE_UNIT ( ) SI_UNIT ( $, .RADIAN. ) );
#2081 = VERTEX_POINT ( 'NONE', #23305 ) ;
#2082 = EDGE_CURVE ( 'NONE', #24246, #19138, #25959, .T. ) ;
#2083 = DIRECTION ( 'NONE',  ( 1.000000000000000000, 0.000000000000000000, 0.000000000000000000 ) ) ;
#2084 = ORIENTED_EDGE ( 'NONE', *, *, #19529, .F. ) ;
#2085 = ADVANCED_FACE ( 'NONE', ( #3611 ), #17365, .F. ) ;
#2086 = DIRECTION ( 'NONE',  ( 0.000000000000000000, -1.000000000000000000, 0.000000000000000000 ) ) ;
#2087 = EDGE_LOOP ( 'NONE', ( #4456, #24594, #552, #27769 ) ) ;
#2088 = AXIS2_PLACEMENT_3D ( 'NONE', #6259, #23790, #2363 ) ;
#2089 = ORIENTED_EDGE ( 'NONE', *, *, #3406, .F. ) ;
#2090 = DIRECTION ( 'NONE',  ( -0.000000000000000000, 0.000000000000000000, -1.000000000000000000 ) ) ;
#2091 = ORIENTED_EDGE ( 'NONE', *, *, #5972, .T. ) ;
#2092 = CIRCLE ( 'NONE', #3938, 5.000000000000004441 ) ;
#2093 = ORIENTED_EDGE ( 'NONE', *, *, #23944, .T. ) ;
#2094 = CARTESIAN_POINT ( 'NONE',  ( -223.0199379110806035, 134.9200334684876168, 15.12837422688625644 ) ) ;
#2095 = CARTESIAN_POINT ( 'NONE',  ( -136.8324479085035250, 127.9412362963770704, -17.51947590493717044 ) ) ;
#2096 = CARTESIAN_POINT ( 'NONE',  ( -213.1248215185737820, -216.9499264940854744, 94.81074245358750829 ) ) ;
#2097 = DIRECTION ( 'NONE',  ( -0.8916010070294605461, -0.4528218681380702382, 0.000000000000000000 ) ) ;
#2098 = DIRECTION ( 'NONE',  ( -1.000000000000000000, 0.000000000000000000, 0.000000000000000000 ) ) ;
#2099 = PLANE ( 'NONE',  #25254 ) ;
#2100 = DIRECTION ( 'NONE',  ( 1.541976423090495387E-16, -1.000000000000000000, 0.000000000000000000 ) ) ;
#2101 = CARTESIAN_POINT ( 'NONE',  ( -209.5896013737285273, 89.20569115677373873, -25.08817329724644551 ) ) ;
#2102 = FACE_OUTER_BOUND ( 'NONE', #2087, .T. ) ;
#2103 = AXIS2_PLACEMENT_3D ( 'NONE', #3755, #21143, #12265 ) ;
#2104 = DIRECTION ( 'NONE',  ( -0.000000000000000000, -1.000000000000000000, -0.000000000000000000 ) ) ;
#2105 = EDGE_CURVE ( 'NONE', #6230, #3625, #10237, .T. ) ;
#2106 = DIRECTION ( 'NONE',  ( 1.000000000000000000, 0.000000000000000000, 0.000000000000000000 ) ) ;
#2107 = FACE_OUTER_BOUND ( 'NONE', #26223, .T. ) ;
#2108 = CARTESIAN_POINT ( 'NONE',  ( 139.9999999999999716, -100.0000000000000000, 70.00000000000001421 ) ) ;
#2109 = VECTOR ( 'NONE', #6827, 1000.000000000000227 ) ;
#2110 = EDGE_LOOP ( 'NONE', ( #12716, #23879, #5558, #10573 ) ) ;
#2111 = DIRECTION ( 'NONE',  ( -0.000000000000000000, 0.000000000000000000, -1.000000000000000000 ) ) ;
#2112 = ADVANCED_FACE ( 'NONE', ( #4297 ), #26126, .F. ) ;
#2113 = LINE ( 'NONE', #10750, #15570 ) ;
#2114 = FACE_BOUND ( 'NONE', #9534, .T. ) ;
#2115 = AXIS2_PLACEMENT_3D ( 'NONE', #26238, #17621, #22363 ) ;
#2116 = ORIENTED_EDGE ( 'NONE', *, *, #5364, .T. ) ;
#2117 = APPLICATION_CONTEXT ( 'automotive_design' ) ;
#2118 = CARTESIAN_POINT ( 'NONE',  ( 87.50000000000012790, 240.0000000000000000, -15.95262490344442874 ) ) ;
#2119 = VERTEX_POINT ( 'NONE', #14274 ) ;
#2120 = EDGE_CURVE ( 'NONE', #4808, #25545, #12669, .T. ) ;
#2121 = DIRECTION ( 'NONE',  ( -0.9659258262890705327, -0.2588190451025121908, 0.000000000000000000 ) ) ;
#2122 = ORIENTED_EDGE ( 'NONE', *, *, #1590, .T. ) ;
#2123 = VERTEX_POINT ( 'NONE', #12124 ) ;
#2124 = EDGE_CURVE ( 'NONE', #22290, #17151, #18849, .T. ) ;
#2125 = ORIENTED_EDGE ( 'NONE', *, *, #4425, .T. ) ;
#2126 = EDGE_LOOP ( 'NONE', ( #10887, #1967, #16409, #23505 ) ) ;
#2127 = CARTESIAN_POINT ( 'NONE',  ( 65.00000000000000000, -150.0000000000000568, -75.99999999999998579 ) ) ;
#2128 = AXIS2_PLACEMENT_3D ( 'NONE', #17004, #16870, #21173 ) ;
#2129 = DIRECTION ( 'NONE',  ( -0.000000000000000000, 1.000000000000000000, -1.387778780781445429E-16 ) ) ;
#2130 = DIRECTION ( 'NONE',  ( -1.000000000000000000, 0.000000000000000000, -9.251858538542972814E-17 ) ) ;
#2131 = CARTESIAN_POINT ( 'NONE',  ( 157.9999999999996589, 279.1890001801680796, 45.00000000000000000 ) ) ;
#2132 = ADVANCED_FACE ( 'NONE', ( #28272 ), #7797, .F. ) ;
#2133 = CARTESIAN_POINT ( 'NONE',  ( -216.3679220181659275, 71.52319660855000905, 25.09443459582798042 ) ) ;
#2134 = DIRECTION ( 'NONE',  ( -0.000000000000000000, -0.000000000000000000, -1.000000000000000000 ) ) ;
#2135 = CARTESIAN_POINT ( 'NONE',  ( -17.24491960465745777, -18.01420295945611727, 100.0000000000000000 ) ) ;
#2136 = CARTESIAN_POINT ( 'NONE',  ( 134.9999999999998579, 404.6636166603179277, -145.0000000000000000 ) ) ;
#2137 = CARTESIAN_POINT ( 'NONE',  ( -143.2374437020967264, 68.51688903468615877, 83.00000000000001421 ) ) ;
#2138 = DIRECTION ( 'NONE',  ( 0.4528218681382319422, 0.8916010070293783896, -0.000000000000000000 ) ) ;
#2139 = CARTESIAN_POINT ( 'NONE',  ( -223.7930071774131022, 71.88803283280797984, -19.06147322994570459 ) ) ;
#2140 = EDGE_CURVE ( 'NONE', #14281, #9708, #7935, .T. ) ;
#2141 = DIRECTION ( 'NONE',  ( 1.000000000000000000, -0.000000000000000000, -0.000000000000000000 ) ) ;
#2142 = CARTESIAN_POINT ( 'NONE',  ( -207.5044420441007560, 75.59897387903042443, 45.00000000000000000 ) ) ;
#2143 = DIRECTION ( 'NONE',  ( -1.000000000000000000, -9.204883169708156517E-49, 3.053113317719176542E-15 ) ) ;
#2144 = DIRECTION ( 'NONE',  ( -0.000000000000000000, 1.000000000000000000, -1.387778780781445429E-16 ) ) ;
#2146 = EDGE_LOOP ( 'NONE', ( #5903, #27907, #19160, #4136 ) ) ;
#2145 = ORIENTED_EDGE ( 'NONE', *, *, #23367, .F. ) ;
#2147 = AXIS2_PLACEMENT_3D ( 'NONE', #7925, #1177, #18702 ) ;
#2148 = CARTESIAN_POINT ( 'NONE',  ( -164.5564299301625226, 118.4912152583887490, 22.95374496050424895 ) ) ;
#2149 = DIRECTION ( 'NONE',  ( 0.8916010070296733758, -0.4528218681376511845, 0.000000000000000000 ) ) ;
#2150 = ORIENTED_EDGE ( 'NONE', *, *, #26551, .F. ) ;
#2151 = SHAPE_DEFINITION_REPRESENTATION ( #25856, #3128 ) ;
#2152 = ORIENTED_EDGE ( 'NONE', *, *, #23804, .T. ) ;
#2153 = EDGE_LOOP ( 'NONE', ( #18531, #17494, #11357, #20141 ) ) ;
#2154 = EDGE_CURVE ( 'NONE', #11738, #18634, #27740, .T. ) ;
#2155 = EDGE_CURVE ( 'NONE', #25901, #13173, #28242, .T. ) ;
#2156 = CARTESIAN_POINT ( 'NONE',  ( -219.9082363642617679, 137.1815813412194700, -12.98324324876687363 ) ) ;
#2157 = FACE_OUTER_BOUND ( 'NONE', #3072, .T. ) ;
#2158 = ORIENTED_EDGE ( 'NONE', *, *, #24799, .T. ) ;
#2159 = CARTESIAN_POINT ( 'NONE',  ( 91.70829090828171104, 81.72138244998292578, -100.0000000000000284 ) ) ;
#2160 = LINE ( 'NONE', #10939, #20589 ) ;
#2161 = ORIENTED_EDGE ( 'NONE', *, *, #12174, .T. ) ;
#2162 = CARTESIAN_POINT ( 'NONE',  ( -214.4302377132927404, 86.70854347113640870, 22.08344159346780344 ) ) ;
#2163 = ORIENTED_EDGE ( 'NONE', *, *, #23541, .F. ) ;
#2164 = AXIS2_PLACEMENT_3D ( 'NONE', #17497, #17357, #21675 ) ;
#2165 = LINE ( 'NONE', #20122, #16244 ) ;
#2166 = ADVANCED_FACE ( 'NONE', ( #14689 ), #9817, .F. ) ;
#2167 = LINE ( 'NONE', #25, #5708 ) ;
#2168 = CARTESIAN_POINT ( 'NONE',  ( -270.1025481742786951, -91.18033988749901653, 0.000000000000000000 ) ) ;
#2169 = EDGE_CURVE ( 'NONE', #27071, #14580, #10770, .T. ) ;
#2170 = ORIENTED_EDGE ( 'NONE', *, *, #26246, .T. ) ;
#2171 = DIRECTION ( 'NONE',  ( -0.4999999999999919509, 0.8660254037844432595, -1.224646799147353207E-16 ) ) ;
#2172 = ADVANCED_FACE ( 'NONE', ( #1186 ), #23024, .F. ) ;
#2173 = DIRECTION ( 'NONE',  ( 1.000000000000000000, -0.000000000000000000, -0.000000000000000000 ) ) ;
#2174 = CARTESIAN_POINT ( 'NONE',  ( -254.3350114625770289, -91.18033988749901653, 0.000000000000000000 ) ) ;
#2175 = LINE ( 'NONE', #17987, #5245 ) ;
#2176 = ORIENTED_EDGE ( 'NONE', *, *, #8706, .F. ) ;
#2177 = CARTESIAN_POINT ( 'NONE',  ( 157.4999999999998579, 45.70268697826052318, 45.00000000000000000 ) ) ;
#2178 = CIRCLE ( 'NONE', #27455, 53.86582179324592090 ) ;
#2179 = FACE_OUTER_BOUND ( 'NONE', #21456, .T. ) ;
#2180 = DIRECTION ( 'NONE',  ( -1.000000000000000000, 0.000000000000000000, 0.000000000000000000 ) ) ;
#2181 = ORIENTED_EDGE ( 'NONE', *, *, #6541, .F. ) ;
#2182 = ORIENTED_EDGE ( 'NONE', *, *, #15398, .F. ) ;
#2183 = DIRECTION ( 'NONE',  ( 1.000000000000000000, -0.000000000000000000, -0.000000000000000000 ) ) ;
#2184 = CARTESIAN_POINT ( 'NONE',  ( -191.3061555549459740, 102.2427340594756799, -32.85867620729514016 ) ) ;
#2185 = ORIENTED_EDGE ( 'NONE', *, *, #19938, .F. ) ;
#2186 = ORIENTED_EDGE ( 'NONE', *, *, #278, .T. ) ;
#2187 = CARTESIAN_POINT ( 'NONE',  ( -110.9204421502694089, 68.96622493949561772, 82.96750001901793325 ) ) ;
#2188 = PLANE ( 'NONE',  #12575 ) ;
#2189 = ORIENTED_EDGE ( 'NONE', *, *, #1216, .T. ) ;
#2190 = EDGE_LOOP ( 'NONE', ( #11825, #16793, #16024, #14263 ) ) ;
#2191 = CARTESIAN_POINT ( 'NONE',  ( -24.75198612830871525, 128.0415922265599988, 17.48639942061494779 ) ) ;
#2192 = VECTOR ( 'NONE', #13945, 1000.000000000000114 ) ;
#2193 = AXIS2_PLACEMENT_3D ( 'NONE', #16157, #9825, #22894 ) ;
#2194 = CARTESIAN_POINT ( 'NONE',  ( 113.4538925329242574, 207.5603490538955782, -145.0000000000000000 ) ) ;
#2195 = FACE_OUTER_BOUND ( 'NONE', #8358, .T. ) ;
#2196 = DIRECTION ( 'NONE',  ( 0.000000000000000000, 0.000000000000000000, -1.000000000000000000 ) ) ;
#2197 = EDGE_CURVE ( 'NONE', #4442, #24279, #18091, .T. ) ;
#2198 = DIRECTION ( 'NONE',  ( 1.000000000000000000, 0.000000000000000000, 0.000000000000000000 ) ) ;
#2199 = ADVANCED_FACE ( 'NONE', ( #24548 ), #17791, .F. ) ;
#2200 = DIRECTION ( 'NONE',  ( 0.000000000000000000, 0.000000000000000000, 1.000000000000000000 ) ) ;
#2201 = DIRECTION ( 'NONE',  ( 0.000000000000000000, 0.7071067811865476838, 0.7071067811865474617 ) ) ;
#2202 = EDGE_LOOP ( 'NONE', ( #8838, #14033, #21840, #5413 ) ) ;
#2203 = DIRECTION ( 'NONE',  ( 0.9985600561963492439, 0.05364526231778202897, 0.000000000000000000 ) ) ;
#2204 = CARTESIAN_POINT ( 'NONE',  ( 134.9999999999998863, 404.6636166603179277, -137.0000000000000000 ) ) ;
#2205 = DIRECTION ( 'NONE',  ( 0.4528218681382519262, -0.8916010070293682865, 0.000000000000000000 ) ) ;
#2206 = DIRECTION ( 'NONE',  ( -0.000000000000000000, -1.000000000000000000, -0.000000000000000000 ) ) ;
#2207 = ORIENTED_EDGE ( 'NONE', *, *, #674, .F. ) ;
#2208 = PLANE ( 'NONE',  #21967 ) ;
#2209 = VECTOR ( 'NONE', #5749, 1000.000000000000000 ) ;
#2210 = DIRECTION ( 'NONE',  ( 1.000000000000000000, -0.000000000000000000, -0.000000000000000000 ) ) ;
#2211 = CARTESIAN_POINT ( 'NONE',  ( -243.4285414610288001, 74.63108012613849951, -5.000000000000003553 ) ) ;
#2212 = CARTESIAN_POINT ( 'NONE',  ( 157.4999999999996305, 283.9508126914284958, -45.00000000000000000 ) ) ;
#2213 = DIRECTION ( 'NONE',  ( 0.8916010070294098089, 0.4528218681381699917, 0.000000000000000000 ) ) ;
#2214 = LINE ( 'NONE', #11000, #23023 ) ;
#2215 = ORIENTED_EDGE ( 'NONE', *, *, #16315, .T. ) ;
#2216 = AXIS2_PLACEMENT_3D ( 'NONE', #2525, #13468, #11754 ) ;
#2217 = CARTESIAN_POINT ( 'NONE',  ( -208.0993096659099706, 75.16660988589454462, 39.82168146137254183 ) ) ;
#2218 = VERTEX_POINT ( 'NONE', #6877 ) ;
#2219 = EDGE_CURVE ( 'NONE', #5556, #2475, #2413, .T. ) ;
#2220 = FACE_OUTER_BOUND ( 'NONE', #11224, .T. ) ;
#2221 = VECTOR ( 'NONE', #20588, 1000.000000000000000 ) ;
#2222 = ORIENTED_EDGE ( 'NONE', *, *, #8741, .F. ) ;
#2223 = ORIENTED_EDGE ( 'NONE', *, *, #794, .T. ) ;
#2224 = DIRECTION ( 'NONE',  ( 0.000000000000000000, 0.000000000000000000, 1.000000000000000000 ) ) ;
#2225 = EDGE_CURVE ( 'NONE', #26896, #21202, #2272, .T. ) ;
#2226 = EDGE_LOOP ( 'NONE', ( #21509, #4971, #16679, #25481, #14713, #23538 ) ) ;
#2227 = VERTEX_POINT ( 'NONE', #19949 ) ;
#2228 = CARTESIAN_POINT ( 'NONE',  ( -226.9194714820147851, 131.5555516077983498, 12.99999999956374275 ) ) ;
#2229 = CARTESIAN_POINT ( 'NONE',  ( 98.85598102459226766, 241.6222630368753528, 21.45481330788183527 ) ) ;
#2230 = VECTOR ( 'NONE', #25058, 1000.000000000000000 ) ;
#2231 = LINE ( 'NONE', #24359, #12852 ) ;
#2232 = ADVANCED_FACE ( 'NONE', ( #15658 ), #421, .F. ) ;
#2233 = DIRECTION ( 'NONE',  ( -0.8916010070295112833, -0.4528218681379702626, 0.000000000000000000 ) ) ;
#2234 = EDGE_CURVE ( 'NONE', #24120, #14926, #7170, .T. ) ;
#2235 = CARTESIAN_POINT ( 'NONE',  ( 111.3836151241014960, 219.3130464734738325, -45.00000000000000000 ) ) ;
#2236 = CIRCLE ( 'NONE', #15547, 9.999999999999991118 ) ;
#2237 = PLANE ( 'NONE',  #21348 ) ;
#2238 = PLANE ( 'NONE',  #28064 ) ;
#2239 = ADVANCED_FACE ( 'NONE', ( #24693 ), #4571, .T. ) ;
#2240 = CARTESIAN_POINT ( 'NONE',  ( 157.4999999999998579, 138.4940622560211239, -45.00000000000000000 ) ) ;
#2241 = CARTESIAN_POINT ( 'NONE',  ( 157.4999999999998579, 183.6358123911478799, 45.00000000000000000 ) ) ;
#2242 = DIRECTION ( 'NONE',  ( 1.000000000000000000, 4.163336342344337027E-16, 0.000000000000000000 ) ) ;
#2243 = CARTESIAN_POINT ( 'NONE',  ( 158.0000000000008527, 125.7007497147323818, 45.00000000000000000 ) ) ;
#2244 = LINE ( 'NONE', #11027, #18518 ) ;
#2245 = VECTOR ( 'NONE', #17439, 1000.000000000000000 ) ;
#2246 = ORIENTED_EDGE ( 'NONE', *, *, #12352, .F. ) ;
#2247 = FACE_OUTER_BOUND ( 'NONE', #3999, .T. ) ;
#2248 = AXIS2_PLACEMENT_3D ( 'NONE', #4320, #595, #24157 ) ;
#2249 = DIRECTION ( 'NONE',  ( 0.000000000000000000, 0.000000000000000000, 1.000000000000000000 ) ) ;
#2250 = DIRECTION ( 'NONE',  ( 1.000000000000000000, 0.000000000000000000, -0.000000000000000000 ) ) ;
#2251 = PLANE ( 'NONE',  #12927 ) ;
#2252 = ORIENTED_EDGE ( 'NONE', *, *, #26243, .F. ) ;
#2253 = VECTOR ( 'NONE', #12899, 1000.000000000000000 ) ;
#2254 = CARTESIAN_POINT ( 'NONE',  ( 109.9730600663540372, 258.3045051371750560, -43.53165882719768831 ) ) ;
#2255 = EDGE_LOOP ( 'NONE', ( #1277, #11284, #6297, #21132 ) ) ;
#2256 = ORIENTED_EDGE ( 'NONE', *, *, #24363, .F. ) ;
#2257 = ORIENTED_EDGE ( 'NONE', *, *, #11814, .T. ) ;
#2258 = AXIS2_PLACEMENT_3D ( 'NONE', #11059, #12938, #28277 ) ;
#2259 = ORIENTED_EDGE ( 'NONE', *, *, #19337, .T. ) ;
#2260 = B_SPLINE_CURVE_WITH_KNOTS ( 'NONE', 3,
 ( #23158, #20993, #8356, #27588, #18985, #27447, #25579, #5906, #7791, #16974, #25726, #6051, #14832, #17116, #23583, #12682, #10509, #25870, #6196, #23721, #5632, #3467, #4031, #14404, #12818, #12257, #9946, #18703, #15113, #20373, #8498, #6330, #21712, #700 ),
 .UNSPECIFIED., .F., .F.,
 ( 4, 2, 2, 2, 2, 2, 2, 2, 2, 2, 2, 2, 2, 2, 2, 2, 4 ),
 ( -3.473018576686760843E-05, 0.003158948505162983023, 0.006352627196092834258, 0.01273998457795253066, 0.01912734195981235022, 0.02232102065074227995, 0.02551469934167219233, 0.03190205672353205180, 0.03509573541446200928, 0.03669257475992701578, 0.03828941410539202228, 0.04148309279632195895, 0.04307993214178691688, 0.04467677148725186786, 0.04627361083271682579, 0.04787045017818177678, 0.05106412886911163712 ),
 .UNSPECIFIED. ) ;
#2261 = ORIENTED_EDGE ( 'NONE', *, *, #16658, .F. ) ;
#2262 = ORIENTED_EDGE ( 'NONE', *, *, #13884, .T. ) ;
#2263 = CARTESIAN_POINT ( 'NONE',  ( -141.6428522700808230, 74.54464929955099706, 83.00000000000001421 ) ) ;
#2264 = AXIS2_PLACEMENT_3D ( 'NONE', #2700, #11190, #6725 ) ;
#2265 = ADVANCED_FACE ( 'NONE', ( #4714 ), #281, .F. ) ;
#2266 = EDGE_CURVE ( 'NONE', #14227, #20107, #3930, .T. ) ;
#2267 = ADVANCED_FACE ( 'NONE', ( #22248 ), #19806, .F. ) ;
#2268 = CARTESIAN_POINT ( 'NONE',  ( 79.99999999999990052, 139.9999999999999716, -15.00000000000000000 ) ) ;
#2269 = LINE ( 'NONE', #6873, #2943 ) ;
#2270 = CARTESIAN_POINT ( 'NONE',  ( -223.4403667166160972, 71.79593500864935152, 19.27754551403305427 ) ) ;
#2271 = CARTESIAN_POINT ( 'NONE',  ( 157.4999999999998579, 153.5413123010633853, 45.00000000000000000 ) ) ;
#2272 = LINE ( 'NONE', #11196, #26887 ) ;
#2273 = VECTOR ( 'NONE', #1585, 1000.000000000000000 ) ;
#2274 = EDGE_CURVE ( 'NONE', #14725, #19755, #13595, .T. ) ;
#2275 = LINE ( 'NONE', #24263, #2562 ) ;
#2276 = LINE ( 'NONE', #21684, #19032 ) ;
#2277 = LINE ( 'NONE', #25988, #14141 ) ;
#2278 = CARTESIAN_POINT ( 'NONE',  ( 9.999999999999749534, 90.00000000000001421, 80.00000000000001421 ) ) ;
#2279 = TOROIDAL_SURFACE ( 'NONE', #22015, 16.91094714394370158, 6.204828372381208546 ) ;
#2280 = CARTESIAN_POINT ( 'NONE',  ( -28.14009829505550542, 129.1550027291188201, 16.99829214959097357 ) ) ;
#2281 = CARTESIAN_POINT ( 'NONE',  ( -209.8597537650321385, 64.07535392826727616, 30.05220721473784806 ) ) ;
#2282 = CARTESIAN_POINT ( 'NONE',  ( 158.0000000000004263, 166.3346248423521274, 45.00000000000000000 ) ) ;
#2283 = LINE ( 'NONE', #19815, #21231 ) ;
#2285 = ORIENTED_EDGE ( 'NONE', *, *, #6104, .T. ) ;
#2284 = ORIENTED_EDGE ( 'NONE', *, *, #18083, .F. ) ;
#2286 = CARTESIAN_POINT ( 'NONE',  ( -181.5195305165591435, 109.0652686644031633, 30.80202506621170855 ) ) ;
#2287 = DIRECTION ( 'NONE',  ( 0.8916010070299267287, -0.4528218681371523058, 0.000000000000000000 ) ) ;
#2288 = ORIENTED_EDGE ( 'NONE', *, *, #3470, .T. ) ;
#2289 = ORIENTED_EDGE ( 'NONE', *, *, #14950, .T. ) ;
#2290 = VERTEX_POINT ( 'NONE', #9182 ) ;
#2291 = DIRECTION ( 'NONE',  ( 1.000000000000000000, 0.000000000000000000, 0.000000000000000000 ) ) ;
#2292 = VECTOR ( 'NONE', #21360, 1000.000000000000000 ) ;
#2293 = FACE_OUTER_BOUND ( 'NONE', #20733, .T. ) ;
#2294 = EDGE_LOOP ( 'NONE', ( #6044, #13039, #1838, #23092 ) ) ;
#2295 = CARTESIAN_POINT ( 'NONE',  ( 87.74278500253673485, 111.0010834410971370, -100.0000000000000284 ) ) ;
#2296 = AXIS2_PLACEMENT_3D ( 'NONE', #27206, #12280, #10255 ) ;
#2297 = EDGE_CURVE ( 'NONE', #6857, #21241, #564, .T. ) ;
#2298 = ADVANCED_FACE ( 'NONE', ( #2706, #19668 ), #7021, .F. ) ;
#2299 = CARTESIAN_POINT ( 'NONE',  ( 232.4999999999996305, 133.0668745871126930, 36.86484227207694886 ) ) ;
#2300 = ORIENTED_EDGE ( 'NONE', *, *, #5170, .T. ) ;
#2301 = CARTESIAN_POINT ( 'NONE',  ( -223.8494703126554271, 88.80400106072828237, 16.69934009789151830 ) ) ;
#2302 = CARTESIAN_POINT ( 'NONE',  ( 232.4999999999996305, 83.06687458711267880, -36.86484227207694175 ) ) ;
#2303 = LINE ( 'NONE', #9071, #27272 ) ;
#2304 = CARTESIAN_POINT ( 'NONE',  ( 157.4557401840683610, 200.1067917919123431, -144.6099047286053576 ) ) ;
#2305 = VERTEX_POINT ( 'NONE', #9328 ) ;
#2306 = EDGE_CURVE ( 'NONE', #11545, #366, #17504, .T. ) ;
#2307 = CIRCLE ( 'NONE', #1842, 4.355764593064429313 ) ;
#2308 = ADVANCED_FACE ( 'NONE', ( #4431 ), #13217, .F. ) ;
#2309 = DIRECTION ( 'NONE',  ( 0.8916010070297643031, -0.4528218681374719945, 0.000000000000000000 ) ) ;
#2310 = B_SPLINE_CURVE_WITH_KNOTS ( 'NONE', 3,
 ( #23603, #10254, #23321, #8376, #12423, #25892, #1482, #21016, #14993, #21160, #23742, #10675, #28177, #8522, #17274, #23889, #1344, #14706, #2461, #28315, #8660, #26447 ),
 .UNSPECIFIED., .F., .F.,
 ( 4, 2, 2, 2, 2, 2, 2, 2, 2, 2, 4 ),
 ( 0.000000000000000000, 0.006532603454143737914, 0.01306520690828747583, 0.01633150863535932917, 0.01959781036243118946, 0.02613041381657490309, 0.02939671554364671480, 0.03266301727071851957, 0.03919562072486217075, 0.04572822417900581499, 0.05226082763314945923 ),
 .UNSPECIFIED. ) ;
#2311 = CARTESIAN_POINT ( 'NONE',  ( -220.9676528974451060, 136.4492860810281343, -15.12837422688741462 ) ) ;
#2312 = CARTESIAN_POINT ( 'NONE',  ( 158.0000000000016485, 48.46449948952110987, 45.00000000000000000 ) ) ;
#2313 = DIRECTION ( 'NONE',  ( -0.000000000000000000, -0.000000000000000000, -1.000000000000000000 ) ) ;
#2314 = ORIENTED_EDGE ( 'NONE', *, *, #16923, .F. ) ;
#2315 = DIRECTION ( 'NONE',  ( -0.8916010070298258094, -0.4528218681373508137, 0.000000000000000000 ) ) ;
#2316 = CIRCLE ( 'NONE', #4166, 6.025000000000002132 ) ;
#2317 = DIRECTION ( 'NONE',  ( 0.000000000000000000, 0.000000000000000000, -1.000000000000000000 ) ) ;
#2318 = CARTESIAN_POINT ( 'NONE',  ( 134.9999999999998579, -327.2004514666934369, -84.99999999999997158 ) ) ;
#2319 = ORIENTED_EDGE ( 'NONE', *, *, #20746, .T. ) ;
#2320 = DIRECTION ( 'NONE',  ( 0.000000000000000000, 0.000000000000000000, 1.000000000000000000 ) ) ;
#2321 = ORIENTED_EDGE ( 'NONE', *, *, #27279, .T. ) ;
#2322 = EDGE_CURVE ( 'NONE', #20571, #1242, #24589, .T. ) ;
#2323 = EDGE_CURVE ( 'NONE', #4885, #25224, #1261, .T. ) ;
#2324 = CARTESIAN_POINT ( 'NONE',  ( 69.99612328191057031, 261.2290884209365345, -45.00000000000000000 ) ) ;
#2325 = CARTESIAN_POINT ( 'NONE',  ( -187.1339768309721876, 105.1645070492825482, -32.59344809072628379 ) ) ;
#2326 = VERTEX_POINT ( 'NONE', #7598 ) ;
#2327 = ORIENTED_EDGE ( 'NONE', *, *, #17388, .T. ) ;
#2328 = DIRECTION ( 'NONE',  ( 1.000000000000000000, 0.000000000000000000, 0.000000000000000000 ) ) ;
#2329 = VECTOR ( 'NONE', #14493, 1000.000000000000000 ) ;
#2330 = LINE ( 'NONE', #11110, #4291 ) ;
#2331 = EDGE_CURVE ( 'NONE', #3986, #10475, #14982, .T. ) ;
#2332 = ORIENTED_EDGE ( 'NONE', *, *, #13602, .F. ) ;
#2333 = ORIENTED_EDGE ( 'NONE', *, *, #19276, .F. ) ;
#2334 = CARTESIAN_POINT ( 'NONE',  ( 158.0000000000006821, 138.7479997597746433, 45.00000000000000000 ) ) ;
#2335 = VECTOR ( 'NONE', #10779, 1000.000000000000000 ) ;
#2336 = DIRECTION ( 'NONE',  ( 0.8660254037844432595, 0.4999999999999919509, -0.000000000000000000 ) ) ;
#2337 = LINE ( 'NONE', #20160, #8911 ) ;
#2338 = LINE ( 'NONE', #11118, #10822 ) ;
#2339 = DIRECTION ( 'NONE',  ( 1.000000000000000000, 0.000000000000000000, -0.000000000000000000 ) ) ;
#2340 = CARTESIAN_POINT ( 'NONE',  ( -210.0005531822249338, 60.15481880046607444, -20.01098946152725944 ) ) ;
#2341 = DIRECTION ( 'NONE',  ( 0.8916010070293409751, 0.4528218681383056610, 0.000000000000000000 ) ) ;
#2342 = VERTEX_POINT ( 'NONE', #5291 ) ;
#2343 = EDGE_CURVE ( 'NONE', #9011, #23606, #20659, .T. ) ;
#2344 = DIRECTION ( 'NONE',  ( -0.8916010070294808632, -0.4528218681380302146, 0.000000000000000000 ) ) ;
#2345 = CARTESIAN_POINT ( 'NONE',  ( 217.4999999999996305, -5.589247009368136787, -100.0000000000000142 ) ) ;
#2346 = DIRECTION ( 'NONE',  ( 0.000000000000000000, 0.000000000000000000, 1.000000000000000000 ) ) ;
#2347 = CARTESIAN_POINT ( 'NONE',  ( 123.9999999999998579, 220.0000000000000284, -100.0000000000000142 ) ) ;
#2348 = ORIENTED_EDGE ( 'NONE', *, *, #21810, .T. ) ;
#2349 = PLANE ( 'NONE',  #8686 ) ;
#2350 = ORIENTED_EDGE ( 'NONE', *, *, #20216, .T. ) ;
#2351 = CIRCLE ( 'NONE', #1432, 72.21503689626329958 ) ;
#2352 = PLANE ( 'NONE',  #12553 ) ;
#2353 = DIRECTION ( 'NONE',  ( 0.000000000000000000, 1.000000000000000000, 0.000000000000000000 ) ) ;
#2354 = CARTESIAN_POINT ( 'NONE',  ( 138.9677719900889770, 249.7377618559918062, -149.5176478624189542 ) ) ;
#2355 = ORIENTED_EDGE ( 'NONE', *, *, #20263, .F. ) ;
#2356 = DIRECTION ( 'NONE',  ( -0.000000000000000000, -0.000000000000000000, -1.000000000000000000 ) ) ;
#2357 = PRESENTATION_STYLE_ASSIGNMENT (( #24209 ) ) ;
#2358 = ORIENTED_EDGE ( 'NONE', *, *, #10579, .F. ) ;
#2359 = CIRCLE ( 'NONE', #18432, 30.00000000000000000 ) ;
#2360 = TOROIDAL_SURFACE ( 'NONE', #9727, 66.76834224489934400, 2.000000000000000000 ) ;
#2361 = LINE ( 'NONE', #22199, #26753 ) ;
#2362 = ORIENTED_EDGE ( 'NONE', *, *, #6195, .F. ) ;
#2363 = DIRECTION ( 'NONE',  ( 0.8916010070293384215, 0.4528218681383106015, 0.000000000000000000 ) ) ;
#2364 = ORIENTED_EDGE ( 'NONE', *, *, #6001, .T. ) ;
#2365 = EDGE_CURVE ( 'NONE', #19653, #17465, #19545, .T. ) ;
#2366 = ORIENTED_EDGE ( 'NONE', *, *, #15464, .T. ) ;
#2367 = EDGE_CURVE ( 'NONE', #19053, #19430, #18514, .T. ) ;
#2368 = CARTESIAN_POINT ( 'NONE',  ( 157.9999999999996589, 281.1890001801680796, 45.00000000000000000 ) ) ;
#2369 = EDGE_CURVE ( 'NONE', #4844, #19307, #27531, .T. ) ;
#2370 = VERTEX_POINT ( 'NONE', #18649 ) ;
#2371 = VERTEX_POINT ( 'NONE', #12057 ) ;
#2372 = CARTESIAN_POINT ( 'NONE',  ( -224.0246150495877089, 134.1142769380900290, 12.98324324887168224 ) ) ;
#2373 = CARTESIAN_POINT ( 'NONE',  ( 87.49999999999988631, 240.0000000000000284, 15.95262490344436479 ) ) ;
#2374 = AXIS2_PLACEMENT_3D ( 'NONE', #11423, #18021, #2070 ) ;
#2375 = CARTESIAN_POINT ( 'NONE',  ( 158.0000000000003695, 173.3503748573662051, 45.00000000000000000 ) ) ;
#2376 = CARTESIAN_POINT ( 'NONE',  ( 158.0000000000003979, 168.8424998498591663, 45.00000000000000000 ) ) ;
#2377 = CIRCLE ( 'NONE', #6507, 14.13483123440684253 ) ;
#2378 = PRODUCT_DEFINITION_FORMATION_WITH_SPECIFIED_SOURCE ( 'ANY', '', #12576, .NOT_KNOWN. ) ;
#2379 = DIRECTION ( 'NONE',  ( 0.8916010070293484135, -0.4528218681382910060, 0.000000000000000000 ) ) ;
#2380 = CARTESIAN_POINT ( 'NONE',  ( 157.4999999999998579, 130.9704372334999789, 45.00000000000000000 ) ) ;
#2381 = CYLINDRICAL_SURFACE ( 'NONE', #5605, 5.000000000000004441 ) ;
#2382 = PLANE ( 'NONE',  #4391 ) ;
#2383 = LINE ( 'NONE', #390, #12473 ) ;
#2384 = FACE_OUTER_BOUND ( 'NONE', #23508, .T. ) ;
#2385 = LINE ( 'NONE', #17911, #6577 ) ;
#2386 = EDGE_LOOP ( 'NONE', ( #20127, #13253, #27932, #9202 ) ) ;
#2387 = FACE_OUTER_BOUND ( 'NONE', #11764, .T. ) ;
#2388 = CARTESIAN_POINT ( 'NONE',  ( 158.0000000000008527, 125.7007497147323818, -45.00000000000000000 ) ) ;
#2389 = CARTESIAN_POINT ( 'NONE',  ( 123.9999999999998579, 220.0000000000000284, 100.0000000000000142 ) ) ;
#2390 = CARTESIAN_POINT ( 'NONE',  ( 108.9212046047250055, 205.1697986248093173, -138.9999999999999432 ) ) ;
#2391 = ORIENTED_EDGE ( 'NONE', *, *, #3143, .T. ) ;
#2392 = VECTOR ( 'NONE', #25105, 1000.000000000000000 ) ;
#2393 = CIRCLE ( 'NONE', #7466, 6.000000000000005329 ) ;
#2394 = CARTESIAN_POINT ( 'NONE',  ( 158.0000000000008242, 126.2086247222394206, 45.00000000000000000 ) ) ;
#2395 = ORIENTED_EDGE ( 'NONE', *, *, #3174, .F. ) ;
#2396 = CARTESIAN_POINT ( 'NONE',  ( -27.08958435577652679, 129.1630609446471283, -15.68767212615508555 ) ) ;
#2397 = ORIENTED_EDGE ( 'NONE', *, *, #1538, .T. ) ;
#2398 = ADVANCED_FACE ( 'NONE', ( #16503 ), #5572, .F. ) ;
#2399 = AXIS2_PLACEMENT_3D ( 'NONE', #6474, #4591, #17246 ) ;
#2400 = ORIENTED_EDGE ( 'NONE', *, *, #10977, .F. ) ;
#2401 = EDGE_CURVE ( 'NONE', #25350, #8917, #22540, .T. ) ;
#2402 = EDGE_CURVE ( 'NONE', #17181, #7680, #13623, .T. ) ;
#2403 = EDGE_CURVE ( 'NONE', #4097, #7691, #23380, .T. ) ;
#2404 = VERTEX_POINT ( 'NONE', #21362 ) ;
#2405 = VERTEX_POINT ( 'NONE', #6138 ) ;
#2406 = CARTESIAN_POINT ( 'NONE',  ( 119.9999999999999432, 2.220446049250311819E-14, -100.0000000000000142 ) ) ;
#2407 = CARTESIAN_POINT ( 'NONE',  ( 158.0000000000016485, 48.46449948952110987, 45.00000000000000000 ) ) ;
#2408 = PLANE ( 'NONE',  #18350 ) ;
#2409 = DIRECTION ( 'NONE',  ( 0.000000000000000000, 0.000000000000000000, -1.000000000000000000 ) ) ;
#2410 = AXIS2_PLACEMENT_3D ( 'NONE', #19417, #16704, #20998 ) ;
#2411 = CARTESIAN_POINT ( 'NONE',  ( -223.4642351922133230, 61.48957812540078294, 20.50364820523368081 ) ) ;
#2412 = DIRECTION ( 'NONE',  ( 0.6681556583950086781, -0.7440215159219069063, 0.000000000000000000 ) ) ;
#2413 = LINE ( 'NONE', #11053, #273 ) ;
#2414 = AXIS2_PLACEMENT_3D ( 'NONE', #575, #22834, #990 ) ;
#2415 = DIRECTION ( 'NONE',  ( 0.8916010070297439860, -0.4528218681375119070, 0.000000000000000000 ) ) ;
#2416 = CARTESIAN_POINT ( 'NONE',  ( -221.3650667873343139, -91.18033988749901653, -19.29759039828519818 ) ) ;
#2417 = VECTOR ( 'NONE', #27846, 1000.000000000000000 ) ;
#2418 = CARTESIAN_POINT ( 'NONE',  ( 157.4999999999998010, 238.8090625563025071, 45.00000000000000000 ) ) ;
#2419 = CARTESIAN_POINT ( 'NONE',  ( -310.0000000000001137, -220.0000000000000853, -59.99999999999987210 ) ) ;
#2420 = AXIS2_PLACEMENT_3D ( 'NONE', #16589, #18182, #27211 ) ;
#2421 = CARTESIAN_POINT ( 'NONE',  ( 4.597555261273185145, 138.9914208893002012, 14.95400808356685829 ) ) ;
#2422 = FACE_OUTER_BOUND ( 'NONE', #26292, .T. ) ;
#2423 = CARTESIAN_POINT ( 'NONE',  ( 157.4999999999998579, 163.5728123310915407, -45.00000000000000000 ) ) ;
#2424 = DIRECTION ( 'NONE',  ( 0.000000000000000000, 0.000000000000000000, 1.000000000000000000 ) ) ;
#2426 = ORIENTED_EDGE ( 'NONE', *, *, #23498, .F. ) ;
#2425 = ORIENTED_EDGE ( 'NONE', *, *, #7125, .F. ) ;
#2427 = CARTESIAN_POINT ( 'NONE',  ( -230.9082317474560284, 90.07627812137737067, -15.14563771791813807 ) ) ;
#2428 = EDGE_CURVE ( 'NONE', #8538, #20676, #17197, .T. ) ;
#2429 = EDGE_CURVE ( 'NONE', #24936, #20648, #8441, .T. ) ;
#2430 = PLANE ( 'NONE',  #21216 ) ;
#2431 = FACE_OUTER_BOUND ( 'NONE', #26216, .T. ) ;
#2432 = EDGE_LOOP ( 'NONE', ( #11207, #2400, #2694, #11717 ) ) ;
#2433 = ORIENTED_EDGE ( 'NONE', *, *, #21835, .T. ) ;
#2434 = AXIS2_PLACEMENT_3D ( 'NONE', #16289, #18295, #25042 ) ;
#2435 = ORIENTED_EDGE ( 'NONE', *, *, #8743, .F. ) ;
#2436 = EDGE_CURVE ( 'NONE', #17217, #19021, #14055, .T. ) ;
#2437 = VECTOR ( 'NONE', #18315, 1000.000000000000000 ) ;
#2438 = CARTESIAN_POINT ( 'NONE',  ( 502.4999999999996021, 494.4107529906318632, -75.35061095560287470 ) ) ;
#2439 = LINE ( 'NONE', #22708, #19095 ) ;
#2440 = EDGE_CURVE ( 'NONE', #13140, #21319, #25669, .T. ) ;
#2441 = ORIENTED_EDGE ( 'NONE', *, *, #26628, .T. ) ;
#2442 = CIRCLE ( 'NONE', #9801, 6.000000000000005329 ) ;
#2443 = DIRECTION ( 'NONE',  ( 1.000000000000000000, 0.000000000000000000, 0.000000000000000000 ) ) ;
#2444 = DIRECTION ( 'NONE',  ( 0.8916010070298759915, -0.4528218681372521703, 0.000000000000000000 ) ) ;
#2445 = VERTEX_POINT ( 'NONE', #23522 ) ;
#2446 = CARTESIAN_POINT ( 'NONE',  ( -225.8597555539711266, 89.56459113752090673, 13.95703860800441198 ) ) ;
#2447 = DIRECTION ( 'NONE',  ( -0.9985600561963481336, 0.05364526231780537141, 0.000000000000000000 ) ) ;
#2448 = DIRECTION ( 'NONE',  ( 0.2845658198851049314, -0.9586565047779721516, 0.000000000000000000 ) ) ;
#2449 = CARTESIAN_POINT ( 'NONE',  ( 157.4819278492304875, 200.1362360204147137, -145.7848141779618629 ) ) ;
#2450 = AXIS2_PLACEMENT_3D ( 'NONE', #27703, #23273, #19099 ) ;
#2451 = ORIENTED_EDGE ( 'NONE', *, *, #8729, .F. ) ;
#2452 = FACE_OUTER_BOUND ( 'NONE', #26418, .T. ) ;
#2453 = ADVANCED_FACE ( 'NONE', ( #8296 ), #5320, .T. ) ;
#2454 = CARTESIAN_POINT ( 'NONE',  ( -270.1025481742786951, -91.18033988749901653, 0.000000000000000000 ) ) ;
#2455 = LINE ( 'NONE', #11241, #12022 ) ;
#2456 = VECTOR ( 'NONE', #2206, 1000.000000000000000 ) ;
#2457 = DIRECTION ( 'NONE',  ( 0.000000000000000000, -1.000000000000000000, 0.000000000000000000 ) ) ;
#2458 = EDGE_LOOP ( 'NONE', ( #3140, #24563, #17382, #22591 ) ) ;
#2459 = DIRECTION ( 'NONE',  ( -0.000000000000000000, -0.000000000000000000, -1.000000000000000000 ) ) ;
#2460 = EDGE_CURVE ( 'NONE', #6964, #22058, #13107, .T. ) ;
#2461 = CARTESIAN_POINT ( 'NONE',  ( -168.2164813390208735, 116.6601697747547774, 24.58600857313708943 ) ) ;
#2462 = CARTESIAN_POINT ( 'NONE',  ( -140.3161500669093300, 71.26253677735444114, 82.82425304866107751 ) ) ;
#2463 = EDGE_LOOP ( 'NONE', ( #27973, #3663, #26251, #20729 ) ) ;
#2464 =( LENGTH_UNIT ( ) NAMED_UNIT ( * ) SI_UNIT ( .MILLI., .METRE. ) );
#2465 = ORIENTED_EDGE ( 'NONE', *, *, #10551, .T. ) ;
#2466 = LINE ( 'NONE', #11255, #21190 ) ;
#2467 = CARTESIAN_POINT ( 'NONE',  ( -203.3278902001933659, 92.92226908766613747, -29.32321494459339561 ) ) ;
#2468 = VERTEX_POINT ( 'NONE', #11311 ) ;
#2469 = VECTOR ( 'NONE', #25107, 1000.000000000000000 ) ;
#2470 = ORIENTED_EDGE ( 'NONE', *, *, #16341, .T. ) ;
#2471 = CARTESIAN_POINT ( 'NONE',  ( 8.415662294793918363, -4.274104551145060604, 45.00000000000000000 ) ) ;
#2472 = EDGE_CURVE ( 'NONE', #9488, #19744, #24227, .T. ) ;
#2473 = CARTESIAN_POINT ( 'NONE',  ( 157.4999999999998579, 48.21056198576756202, 45.00000000000000000 ) ) ;
#2474 = ORIENTED_EDGE ( 'NONE', *, *, #4505, .T. ) ;
#2475 = VERTEX_POINT ( 'NONE', #2380 ) ;
#2476 = VECTOR ( 'NONE', #18133, 1000.000000000000000 ) ;
#2477 = CARTESIAN_POINT ( 'NONE',  ( -4.673085614201822224, 132.3311587643906080, 15.99381942260592915 ) ) ;
#2478 = CARTESIAN_POINT ( 'NONE',  ( 0.3651377029009472142, 1.249999999999999556, -7.402212548643259282 ) ) ;
#2479 = LINE ( 'NONE', #24618, #2006 ) ;
#2480 = CARTESIAN_POINT ( 'NONE',  ( -4.177201536621815592, 134.2095850109177775, -15.52423248666405620 ) ) ;
#2481 = CARTESIAN_POINT ( 'NONE',  ( 157.4999999999998579, 148.5255622860493077, 45.00000000000000000 ) ) ;
#2482 = EDGE_CURVE ( 'NONE', #7477, #12854, #26372, .T. ) ;
#2483 = PLANE ( 'NONE',  #10574 ) ;
#2484 = DIRECTION ( 'NONE',  ( 0.000000000000000000, 1.272130549049657961E-16, -1.000000000000000000 ) ) ;
#2485 = VERTEX_POINT ( 'NONE', #11160 ) ;
#2486 = PLANE ( 'NONE',  #26428 ) ;
#2487 = DIRECTION ( 'NONE',  ( -0.8916010070293711731, 0.4528218681382463751, 0.000000000000000000 ) ) ;
#2488 = CARTESIAN_POINT ( 'NONE',  ( -71.37541315349507443, 150.2892445414773590, 15.00000000000000000 ) ) ;
#2489 = LINE ( 'NONE', #355, #13034 ) ;
#2490 = ORIENTED_EDGE ( 'NONE', *, *, #5540, .T. ) ;
#2491 = VECTOR ( 'NONE', #16396, 1000.000000000000000 ) ;
#2492 = PLANE ( 'NONE',  #18775 ) ;
#2493 = ORIENTED_EDGE ( 'NONE', *, *, #5631, .F. ) ;
#2494 = ADVANCED_FACE ( 'NONE', ( #19915 ), #25006, .T. ) ;
#2495 = CARTESIAN_POINT ( 'NONE',  ( 232.4999999999996305, 83.06687458711267880, 36.86484227207694175 ) ) ;
#2496 = CARTESIAN_POINT ( 'NONE',  ( -227.3759666274727635, 63.27997354833448185, -7.997465051287307780 ) ) ;
#2497 = CARTESIAN_POINT ( 'NONE',  ( 140.0958819112771891, 249.5642367155375041, -141.8266621613457801 ) ) ;
#2498 = ORIENTED_EDGE ( 'NONE', *, *, #19631, .F. ) ;
#2499 = LINE ( 'NONE', #11289, #12946 ) ;
#2500 = VECTOR ( 'NONE', #3983, 1000.000000000000114 ) ;
#2501 = VERTEX_POINT ( 'NONE', #26654 ) ;
#2502 = DIRECTION ( 'NONE',  ( -1.321694076934710155E-16, 1.000000000000000000, 0.000000000000000000 ) ) ;
#2503 = ORIENTED_EDGE ( 'NONE', *, *, #5389, .T. ) ;
#2504 = CARTESIAN_POINT ( 'NONE',  ( 106.4997226413335767, 248.6818526014546933, 25.16395533540803697 ) ) ;
#2505 = EDGE_LOOP ( 'NONE', ( #25413, #21714, #11992, #1413 ) ) ;
#2506 = ORIENTED_EDGE ( 'NONE', *, *, #14809, .F. ) ;
#2507 = ADVANCED_FACE ( 'NONE', ( #21795 ), #2237, .F. ) ;
#2508 = FACE_BOUND ( 'NONE', #21235, .T. ) ;
#2509 = ORIENTED_EDGE ( 'NONE', *, *, #18393, .F. ) ;
#2510 = EDGE_CURVE ( 'NONE', #26112, #27164, #15341, .T. ) ;
#2511 = ORIENTED_EDGE ( 'NONE', *, *, #17869, .T. ) ;
#2512 = ORIENTED_EDGE ( 'NONE', *, *, #21278, .F. ) ;
#2513 = AXIS2_PLACEMENT_3D ( 'NONE', #27989, #16672, #14520 ) ;
#2514 = CARTESIAN_POINT ( 'NONE',  ( 100.3999191023796129, 235.3978472240583528, 22.98606999220467628 ) ) ;
#2515 = LINE ( 'NONE', #26504, #232 ) ;
#2516 = CARTESIAN_POINT ( 'NONE',  ( 158.0000000000003695, 171.3503748573662051, 45.00000000000000000 ) ) ;
#2517 = CIRCLE ( 'NONE', #6650, 29.99999999999999645 ) ;
#2518 = EDGE_CURVE ( 'NONE', #4042, #12076, #28372, .T. ) ;
#2519 = LINE ( 'NONE', #2235, #916 ) ;
#2520 = CARTESIAN_POINT ( 'NONE',  ( 158.0000000000005684, 151.2873747973098659, 45.00000000000000000 ) ) ;
#2521 = DIRECTION ( 'NONE',  ( 3.469446951953614189E-16, -1.000000000000000000, 0.000000000000000000 ) ) ;
#2522 = LINE ( 'NONE', #20055, #15925 ) ;
#2523 = CARTESIAN_POINT ( 'NONE',  ( 158.0000000000004547, 163.8267498348450886, -45.00000000000000000 ) ) ;
#2524 = DIRECTION ( 'NONE',  ( -0.000000000000000000, -0.000000000000000000, -1.000000000000000000 ) ) ;
#2525 = CARTESIAN_POINT ( 'NONE',  ( 367.4999999999996021, -5.589247009368149222, 1.243177022048955014E-14 ) ) ;
#2526 = LINE ( 'NONE', #11317, #4741 ) ;
#2527 = EDGE_CURVE ( 'NONE', #9488, #23090, #13611, .T. ) ;
#2528 = EDGE_LOOP ( 'NONE', ( #4936, #24683, #23676, #15932 ) ) ;
#2529 = DIRECTION ( 'NONE',  ( -0.000000000000000000, 0.000000000000000000, -1.000000000000000000 ) ) ;
#2530 = EDGE_CURVE ( 'NONE', #20966, #20254, #4399, .T. ) ;
#2531 = DIRECTION ( 'NONE',  ( 0.8916010070295316003, 0.4528218681379303501, 0.000000000000000000 ) ) ;
#2532 = LINE ( 'NONE', #22518, #11233 ) ;
#2533 = AXIS2_PLACEMENT_3D ( 'NONE', #12161, #19311, #8400 ) ;
#2534 = EDGE_CURVE ( 'NONE', #26994, #7257, #97, .T. ) ;
#2535 = PLANE ( 'NONE',  #5122 ) ;
#2536 = ORIENTED_EDGE ( 'NONE', *, *, #27938, .T. ) ;
#2537 = CIRCLE ( 'NONE', #19975, 6.025000000000002132 ) ;
#2538 = VECTOR ( 'NONE', #14754, 1000.000000000000000 ) ;
#2539 = DIRECTION ( 'NONE',  ( -0.8916010070293783896, 0.4528218681382319422, 0.000000000000000000 ) ) ;
#2540 = ORIENTED_EDGE ( 'NONE', *, *, #25553, .F. ) ;
#2541 = PLANE ( 'NONE',  #19229 ) ;
#2542 = ORIENTED_EDGE ( 'NONE', *, *, #24570, .T. ) ;
#2543 = AXIS2_PLACEMENT_3D ( 'NONE', #15014, #19732, #24191 ) ;
#2544 = ORIENTED_EDGE ( 'NONE', *, *, #9974, .F. ) ;
#2545 = VERTEX_POINT ( 'NONE', #11021 ) ;
#2546 = EDGE_CURVE ( 'NONE', #17690, #17812, #22215, .T. ) ;
#2547 = ORIENTED_EDGE ( 'NONE', *, *, #10246, .T. ) ;
#2548 = VERTEX_POINT ( 'NONE', #2520 ) ;
#2549 = EDGE_LOOP ( 'NONE', ( #25187, #4897, #16302, #11872 ) ) ;
#2550 = DIRECTION ( 'NONE',  ( 1.000000000000000000, 0.000000000000000000, 0.000000000000000000 ) ) ;
#2551 = CARTESIAN_POINT ( 'NONE',  ( 157.4999999999997726, 246.3326875788235384, -45.00000000000000000 ) ) ;
#2552 = CARTESIAN_POINT ( 'NONE',  ( 158.0000000000009948, 110.6534996696901345, 45.00000000000000000 ) ) ;
#2553 = VECTOR ( 'NONE', #18994, 1000.000000000000227 ) ;
#2554 = UNCERTAINTY_MEASURE_WITH_UNIT (LENGTH_MEASURE( 1.000000000000000082E-05 ), #11582, 'distance_accuracy_value', 'NONE');
#2555 = AXIS2_PLACEMENT_3D ( 'NONE', #17000, #3360, #27765 ) ;
#2556 = DIRECTION ( 'NONE',  ( -0.000000000000000000, -0.000000000000000000, 1.000000000000000000 ) ) ;
#2557 = CARTESIAN_POINT ( 'NONE',  ( -213.5622695550087258, 60.06483686772712360, 14.69413405016535989 ) ) ;
#2558 = DIRECTION ( 'NONE',  ( 0.3102637045530588500, -0.9506505318133536830, 0.000000000000000000 ) ) ;
#2559 = CARTESIAN_POINT ( 'NONE',  ( 157.4999999999998579, 75.79718706834503905, 45.00000000000000000 ) ) ;
#2560 = DIRECTION ( 'NONE',  ( 1.000000000000000000, 0.000000000000000000, -0.000000000000000000 ) ) ;
#2561 = DIRECTION ( 'NONE',  ( 0.8916010070293383105, -0.4528218681383106015, 0.000000000000000000 ) ) ;
#2562 = VECTOR ( 'NONE', #2415, 1000.000000000000227 ) ;
#2563 = DIRECTION ( 'NONE',  ( 0.000000000000000000, 0.000000000000000000, -1.000000000000000000 ) ) ;
#2564 = LINE ( 'NONE', #426, #825 ) ;
#2565 = CARTESIAN_POINT ( 'NONE',  ( 109.5756401952765486, 134.3783162856070703, 89.68749999971406339 ) ) ;
#2566 = ADVANCED_FACE ( 'NONE', ( #24094 ), #8859, .T. ) ;
#2567 = EDGE_CURVE ( 'NONE', #8949, #19837, #20429, .T. ) ;
#2568 = CARTESIAN_POINT ( 'NONE',  ( 157.4999999999998579, 70.78143705333094715, -45.00000000000000000 ) ) ;
#2569 = CARTESIAN_POINT ( 'NONE',  ( 157.9999999999998863, 218.4921249924925348, 45.00000000000000000 ) ) ;
#2570 = DIRECTION ( 'NONE',  ( -0.000000000000000000, -0.000000000000000000, -1.000000000000000000 ) ) ;
#2571 = DIRECTION ( 'NONE',  ( -0.8660254037844394848, 0.4999999999999985012, 0.000000000000000000 ) ) ;
#2573 = EDGE_LOOP ( 'NONE', ( #3042, #14337, #8142, #14582, #16339, #2285, #2327, #26159 ) ) ;
#2572 = ORIENTED_EDGE ( 'NONE', *, *, #18724, .F. ) ;
#2574 = CARTESIAN_POINT ( 'NONE',  ( -204.3509971620249246, 91.62525467510273813, -29.24375089551106299 ) ) ;
#2575 = FACE_OUTER_BOUND ( 'NONE', #5410, .T. ) ;
#2576 = CARTESIAN_POINT ( 'NONE',  ( -203.8386979721259422, 92.04489626552744141, -29.52689898475847485 ) ) ;
#2577 = ORIENTED_EDGE ( 'NONE', *, *, #27411, .F. ) ;
#2578 = CONTEXT_DEPENDENT_SHAPE_REPRESENTATION ( #3038, #16915 ) ;
#2579 = EDGE_LOOP ( 'NONE', ( #9769, #6866, #219 ) ) ;
#2580 = AXIS2_PLACEMENT_3D ( 'NONE', #15107, #13103, #3886 ) ;
#2581 = ORIENTED_EDGE ( 'NONE', *, *, #25702, .T. ) ;
#2582 = CARTESIAN_POINT ( 'NONE',  ( 158.0000000000011653, 95.60624962464788723, 45.00000000000000000 ) ) ;
#2583 = DIRECTION ( 'NONE',  ( 0.8916010070293584056, -0.4528218681382712996, 0.000000000000000000 ) ) ;
#2584 = ADVANCED_FACE ( 'NONE', ( #15769 ), #8719, .F. ) ;
#2585 = VERTEX_POINT ( 'NONE', #6563 ) ;
#2586 = CIRCLE ( 'NONE', #20946, 1.999999999999998890 ) ;
#2587 = ORIENTED_EDGE ( 'NONE', *, *, #26111, .F. ) ;
#2588 = LINE ( 'NONE', #11370, #27832 ) ;
#2589 = EDGE_CURVE ( 'NONE', #3747, #14397, #21824, .T. ) ;
#2590 = CARTESIAN_POINT ( 'NONE',  ( -202.3849748766693892, 93.73600923071712998, -29.14529524674100003 ) ) ;
#2591 = EDGE_LOOP ( 'NONE', ( #12892, #8005, #27859, #10565, #27979 ) ) ;
#2592 = CARTESIAN_POINT ( 'NONE',  ( 161.2365440327092472, 161.2365440327092472, 45.00000000000000000 ) ) ;
#2593 = CARTESIAN_POINT ( 'NONE',  ( -213.1248215185737820, -216.9499264940855028, 105.1892575464125770 ) ) ;
#2594 = CARTESIAN_POINT ( 'NONE',  ( 199.9999999999997726, 0.000000000000000000, -110.0000000000000284 ) ) ;
#2595 = EDGE_CURVE ( 'NONE', #16577, #4345, #812, .T. ) ;
#2596 = DIRECTION ( 'NONE',  ( -1.850371707708594316E-16, 1.000000000000000000, 0.000000000000000000 ) ) ;
#2597 = VECTOR ( 'NONE', #8108, 1000.000000000000000 ) ;
#2598 = CARTESIAN_POINT ( 'NONE',  ( -206.8153965817337223, 60.16463287088505751, -19.99797379519590379 ) ) ;
#2599 = EDGE_CURVE ( 'NONE', #26389, #3911, #9715, .T. ) ;
#2600 = ORIENTED_EDGE ( 'NONE', *, *, #12084, .T. ) ;
#2601 = LINE ( 'NONE', #9651, #18752 ) ;
#2602 = ADVANCED_FACE ( 'NONE', ( #11748 ), #18342, .F. ) ;
#2603 = DIRECTION ( 'NONE',  ( 0.000000000000000000, -1.000000000000000000, 0.000000000000000000 ) ) ;
#2604 = LINE ( 'NONE', #15847, #15708 ) ;
#2605 = DIRECTION ( 'NONE',  ( 1.000000000000000000, 1.657962687179363279E-15, 0.000000000000000000 ) ) ;
#2606 = EDGE_LOOP ( 'NONE', ( #8460, #6398, #1942, #7606 ) ) ;
#2607 = CARTESIAN_POINT ( 'NONE',  ( 158.0000000000016769, 45.95662448201407102, 45.00000000000000000 ) ) ;
#2608 = DIRECTION ( 'NONE',  ( -1.000000000000000000, -0.000000000000000000, 2.775557561562887407E-16 ) ) ;
#2609 = CARTESIAN_POINT ( 'NONE',  ( 158.0000000000005969, 150.7794997898028271, 45.00000000000000000 ) ) ;
#2610 = EDGE_LOOP ( 'NONE', ( #18879, #22337, #17926, #19287 ) ) ;
#2611 = VERTEX_POINT ( 'NONE', #23070 ) ;
#2612 = CARTESIAN_POINT ( 'NONE',  ( 119.4436508138959567, 203.0294372515225518, -45.00000000000000000 ) ) ;
#2613 = CARTESIAN_POINT ( 'NONE',  ( 157.9999999999997158, 256.6181251126050711, -45.00000000000000000 ) ) ;
#2614 = VERTEX_POINT ( 'NONE', #18479 ) ;
#2615 = AXIS2_PLACEMENT_3D ( 'NONE', #5318, #16666, #9920 ) ;
#2616 = ORIENTED_EDGE ( 'NONE', *, *, #4768, .F. ) ;
#2617 = LINE ( 'NONE', #11833, #17754 ) ;
#2618 = VECTOR ( 'NONE', #17782, 1000.000000000000227 ) ;
#2619 = DIRECTION ( 'NONE',  ( -0.000000000000000000, -0.000000000000000000, -1.000000000000000000 ) ) ;
#2620 = ORIENTED_EDGE ( 'NONE', *, *, #8426, .T. ) ;
#2621 = DIRECTION ( 'NONE',  ( -0.000000000000000000, -1.000000000000000000, -0.000000000000000000 ) ) ;
#2622 = EDGE_LOOP ( 'NONE', ( #6693, #15964, #9841, #25577 ) ) ;
#2623 = CARTESIAN_POINT ( 'NONE',  ( -38.51941377410816614, 128.7763188256022318, 17.17685746774373357 ) ) ;
#2624 = ADVANCED_FACE ( 'NONE', ( #5396 ), #9441, .F. ) ;
#2625 = CARTESIAN_POINT ( 'NONE',  ( -260.0000000000001137, -170.0000000000001137, 60.00000000000002132 ) ) ;
#2626 = LINE ( 'NONE', #2772, #22679 ) ;
#2627 = CARTESIAN_POINT ( 'NONE',  ( -31.54578268729987656, 129.2273646750841181, -15.65862884027403190 ) ) ;
#2628 = DIRECTION ( 'NONE',  ( 0.000000000000000000, 0.000000000000000000, -1.000000000000000000 ) ) ;
#2629 = LINE ( 'NONE', #18579, #19751 ) ;
#2630 = DIRECTION ( 'NONE',  ( -0.8660254037844362651, 0.5000000000000039968, -0.000000000000000000 ) ) ;
#2631 = AXIS2_PLACEMENT_3D ( 'NONE', #16120, #11677, #24731 ) ;
#2632 = ORIENTED_EDGE ( 'NONE', *, *, #22566, .F. ) ;
#2633 = LINE ( 'NONE', #27057, #8637 ) ;
#2634 = ADVANCED_FACE ( 'NONE', ( #26951 ), #22652, .T. ) ;
#2635 = B_SPLINE_CURVE_WITH_KNOTS ( 'NONE', 3,
 ( #6213, #1753, #10388, #14703, #27471, #25744, #6072, #10531 ),
 .UNSPECIFIED., .F., .F.,
 ( 4, 2, 2, 4 ),
 ( 0.000000000000000000, 0.003477520733619417822, 0.005216281100429110036, 0.006955041467238803551 ),
 .UNSPECIFIED. ) ;
#2636 = CARTESIAN_POINT ( 'NONE',  ( 158.0000000000013074, 83.06687458711267880, -45.00000000000000000 ) ) ;
#2637 = DIRECTION ( 'NONE',  ( -0.000000000000000000, 0.000000000000000000, -1.000000000000000000 ) ) ;
#2638 = CARTESIAN_POINT ( 'NONE',  ( 157.9999999999996589, 271.6653751576470768, 45.00000000000000000 ) ) ;
#2639 = AXIS2_PLACEMENT_3D ( 'NONE', #16359, #23239, #27115 ) ;
#2640 = VERTEX_POINT ( 'NONE', #25218 ) ;
#2641 = CARTESIAN_POINT ( 'NONE',  ( -220.3653290071073059, 61.04242272473437936, 10.83006322850142311 ) ) ;
#2642 = ORIENTED_EDGE ( 'NONE', *, *, #7765, .T. ) ;
#2643 = EDGE_CURVE ( 'NONE', #14501, #16770, #18055, .T. ) ;
#2644 = DIRECTION ( 'NONE',  ( -0.8916010070293783896, 0.4528218681382319422, 0.000000000000000000 ) ) ;
#2645 = FACE_OUTER_BOUND ( 'NONE', #28388, .T. ) ;
#2646 = CARTESIAN_POINT ( 'NONE',  ( 138.6614742573536887, 249.7775121908574079, -140.2307156351394895 ) ) ;
#2647 = VERTEX_POINT ( 'NONE', #13904 ) ;
#2648 = CARTESIAN_POINT ( 'NONE',  ( 157.9999999999998010, 234.0472500450420341, 45.00000000000000000 ) ) ;
#2649 = CARTESIAN_POINT ( 'NONE',  ( 217.4999999999996305, 83.06687458711267880, 42.86484227207692754 ) ) ;
#2650 = ORIENTED_EDGE ( 'NONE', *, *, #12288, .T. ) ;
#2651 = CARTESIAN_POINT ( 'NONE',  ( -208.9953786179366091, 74.56197851221769213, 36.88754066616979799 ) ) ;
#2652 = ORIENTED_EDGE ( 'NONE', *, *, #27128, .F. ) ;
#2653 = DIRECTION ( 'NONE',  ( 0.8916010070293584056, 0.4528218681382713551, 0.000000000000000000 ) ) ;
#2654 = ORIENTED_EDGE ( 'NONE', *, *, #23931, .T. ) ;
#2655 = EDGE_CURVE ( 'NONE', #23386, #26778, #26812, .T. ) ;
#2656 = ORIENTED_EDGE ( 'NONE', *, *, #27980, .T. ) ;
#2657 = DIRECTION ( 'NONE',  ( 1.000000000000000000, -0.000000000000000000, -0.000000000000000000 ) ) ;
#2658 = ORIENTED_EDGE ( 'NONE', *, *, #3507, .F. ) ;
#2659 = VECTOR ( 'NONE', #22110, 1000.000000000000000 ) ;
#2660 = ORIENTED_EDGE ( 'NONE', *, *, #8195, .T. ) ;
#2661 = VERTEX_POINT ( 'NONE', #1087 ) ;
#2662 = CARTESIAN_POINT ( 'NONE',  ( 96.75280658369925391, 240.7143248587420317, 19.91790936282351865 ) ) ;
#2663 = EDGE_CURVE ( 'NONE', #17425, #12131, #7147, .T. ) ;
#2664 = APPLICATION_CONTEXT ( 'automotive_design' ) ;
#2665 = CARTESIAN_POINT ( 'NONE',  ( 5.999999999999998224, 0.000000000000000000, 0.000000000000000000 ) ) ;
#2666 = DIRECTION ( 'NONE',  ( 0.2066290158914672881, 0.9784193629480785193, 0.000000000000000000 ) ) ;
#2667 = CARTESIAN_POINT ( 'NONE',  ( -63.57415822541634043, -18.01420295945611727, 80.00000000000001421 ) ) ;
#2668 = DIRECTION ( 'NONE',  ( 0.4528218681377111920, 0.8916010070296429557, -0.000000000000000000 ) ) ;
#2669 = DIRECTION ( 'NONE',  ( -1.000000000000000000, 0.000000000000000000, 0.000000000000000000 ) ) ;
#2670 = FACE_OUTER_BOUND ( 'NONE', #9794, .T. ) ;
#2671 = DIRECTION ( 'NONE',  ( 1.321694076934710155E-16, -1.000000000000000000, 0.000000000000000000 ) ) ;
#2672 = CARTESIAN_POINT ( 'NONE',  ( 6.071532165918828775E-15, -70.00000000000002842, -25.00000000000000000 ) ) ;
#2673 = CARTESIAN_POINT ( 'NONE',  ( -196.7918453702777128, 68.51688903468615877, 83.00000000000001421 ) ) ;
#2674 = CARTESIAN_POINT ( 'NONE',  ( 134.9999999999998579, 220.0000000000000284, 100.0000000000000142 ) ) ;
#2675 = VERTEX_POINT ( 'NONE', #5537 ) ;
#2676 = CARTESIAN_POINT ( 'NONE',  ( -277.2150368962633706, -237.2150368962634559, 95.00000000000004263 ) ) ;
#2677 = AXIS2_PLACEMENT_3D ( 'NONE', #19216, #27958, #8304 ) ;
#2678 = EDGE_CURVE ( 'NONE', #26178, #16274, #14311, .T. ) ;
#2679 = EDGE_CURVE ( 'NONE', #24350, #28016, #12165, .T. ) ;
#2680 = CIRCLE ( 'NONE', #25623, 10.71881775658151170 ) ;
#2681 = LINE ( 'NONE', #5123, #20173 ) ;
#2682 = DIRECTION ( 'NONE',  ( -0.5790253867566337309, -0.8153095126952284444, -1.131469241487697676E-14 ) ) ;
#2683 = DIRECTION ( 'NONE',  ( 0.8916010070297244461, 0.4528218681375507093, 0.000000000000000000 ) ) ;
#2684 = ORIENTED_EDGE ( 'NONE', *, *, #17239, .F. ) ;
#2685 = DIRECTION ( 'NONE',  ( 0.4528218681376112720, -0.8916010070296936929, 0.000000000000000000 ) ) ;
#2686 = ORIENTED_EDGE ( 'NONE', *, *, #1570, .F. ) ;
#2687 = DIRECTION ( 'NONE',  ( -0.000000000000000000, -0.000000000000000000, -1.000000000000000000 ) ) ;
#2688 = EDGE_CURVE ( 'NONE', #12924, #9277, #25082, .T. ) ;
#2689 = ORIENTED_EDGE ( 'NONE', *, *, #2015, .F. ) ;
#2690 = EDGE_CURVE ( 'NONE', #8556, #9050, #1228, .T. ) ;
#2691 = VECTOR ( 'NONE', #2141, 1000.000000000000000 ) ;
#2692 = ORIENTED_EDGE ( 'NONE', *, *, #7895, .F. ) ;
#2693 = ORIENTED_EDGE ( 'NONE', *, *, #24007, .F. ) ;
#2694 = ORIENTED_EDGE ( 'NONE', *, *, #22102, .F. ) ;
#2695 = CARTESIAN_POINT ( 'NONE',  ( -86.54034876329639303, 136.4599515387363624, 13.48322035540682151 ) ) ;
#2696 = CARTESIAN_POINT ( 'NONE',  ( 158.0000000000016485, 50.46449948952111697, 45.00000000000000000 ) ) ;
#2697 = LINE ( 'NONE', #24831, #15278 ) ;
#2698 = VECTOR ( 'NONE', #25850, 1000.000000000000000 ) ;
#2699 = AXIS2_PLACEMENT_3D ( 'NONE', #5745, #23135, #25425 ) ;
#2700 = CARTESIAN_POINT ( 'NONE',  ( -210.0000000000000284, -3.238150488490040751E-14, 100.0000000000000142 ) ) ;
#2701 = EDGE_CURVE ( 'NONE', #26144, #23757, #7603, .T. ) ;
#2702 = CARTESIAN_POINT ( 'NONE',  ( 157.9999999999998863, 218.4921249924925348, -45.00000000000000000 ) ) ;
#2703 = AXIS2_PLACEMENT_3D ( 'NONE', #17117, #10232, #25727 ) ;
#2704 = CARTESIAN_POINT ( 'NONE',  ( -225.5840809296988141, 72.49952595023175661, 18.07266724760005516 ) ) ;
#2705 = DIRECTION ( 'NONE',  ( 0.8916010070295817824, -0.4528218681378317623, 0.000000000000000000 ) ) ;
#2706 = FACE_BOUND ( 'NONE', #16319, .T. ) ;
#2707 = CARTESIAN_POINT ( 'NONE',  ( -175.0000000000000000, -170.0000000000001705, 64.00000000000004263 ) ) ;
#2708 = CARTESIAN_POINT ( 'NONE',  ( -215.2757279354555919, 87.86214960428041820, -19.31485547342763098 ) ) ;
#2709 = DIRECTION ( 'NONE',  ( 0.8916010070294598799, -0.4528218681380714594, 0.000000000000000000 ) ) ;
#2710 = CARTESIAN_POINT ( 'NONE',  ( 122.8247714198256944, 204.1329331941749672, 45.00000000000000000 ) ) ;
#2711 = FACE_OUTER_BOUND ( 'NONE', #28224, .T. ) ;
#2713 = DIRECTION ( 'NONE',  ( 1.000000000000000000, 0.000000000000000000, 0.000000000000000000 ) ) ;
#2712 = VECTOR ( 'NONE', #22898, 999.9999999999998863 ) ;
#2714 = CARTESIAN_POINT ( 'NONE',  ( -2.862293735361731706E-14, 109.9999999999999858, 100.0000000000000142 ) ) ;
#2715=STYLED_ITEM('',(#28420),#27732);
#2716 = CARTESIAN_POINT ( 'NONE',  ( 79.99999999999992895, 240.0000000000000284, 45.00000000000000000 ) ) ;
#2717 = DIRECTION ( 'NONE',  ( -0.000000000000000000, 0.000000000000000000, 1.000000000000000000 ) ) ;
#2719 = ORIENTED_EDGE ( 'NONE', *, *, #19437, .F. ) ;
#2718 = ORIENTED_EDGE ( 'NONE', *, *, #708, .F. ) ;
#2720 = CARTESIAN_POINT ( 'NONE',  ( 109.9999999999998863, 330.0000000000000000, 90.00000000000002842 ) ) ;
#2721 = VECTOR ( 'NONE', #7878, 1000.000000000000000 ) ;
#2722 = LINE ( 'NONE', #15961, #25807 ) ;
#2723 = VERTEX_POINT ( 'NONE', #3233 ) ;
#2724 = ORIENTED_EDGE ( 'NONE', *, *, #25952, .F. ) ;
#2726 = VERTEX_POINT ( 'NONE', #12019 ) ;
#2725 = VECTOR ( 'NONE', #21249, 999.9999999999998863 ) ;
#2727 = LINE ( 'NONE', #24857, #11603 ) ;
#2728 = CARTESIAN_POINT ( 'NONE',  ( -149.5659937850672634, 124.9543708090996574, 17.81989871787508051 ) ) ;
#2729 = ORIENTED_EDGE ( 'NONE', *, *, #25118, .T. ) ;
#2730 = EDGE_LOOP ( 'NONE', ( #18731, #8266, #3213, #4515 ) ) ;
#2731 = DIRECTION ( 'NONE',  ( 0.4528218681381114274, 0.8916010070294396739, -0.000000000000000000 ) ) ;
#2732 = ADVANCED_FACE ( 'NONE', ( #20765 ), #9855, .F. ) ;
#2733 = VECTOR ( 'NONE', #15131, 1000.000000000000000 ) ;
#2734 = CARTESIAN_POINT ( 'NONE',  ( -199.9534965974906697, 95.77273073869348252, -30.16924269412446336 ) ) ;
#2735 = ORIENTED_EDGE ( 'NONE', *, *, #11773, .T. ) ;
#2736 = CARTESIAN_POINT ( 'NONE',  ( -203.2481855153401966, 92.57460631283321106, 29.78692811926997663 ) ) ;
#2737 = DIRECTION ( 'NONE',  ( -0.000000000000000000, -0.000000000000000000, 1.000000000000000000 ) ) ;
#2738 = VECTOR ( 'NONE', #20211, 1000.000000000000000 ) ;
#2739 = DIRECTION ( 'NONE',  ( 0.000000000000000000, 0.000000000000000000, -1.000000000000000000 ) ) ;
#2740 = CARTESIAN_POINT ( 'NONE',  ( 65.00000000000000000, -170.0000000000000568, 70.00000000000001421 ) ) ;
#2741 = CARTESIAN_POINT ( 'NONE',  ( -213.6504899993060747, 58.00877466446873143, -34.94433424773174579 ) ) ;
#2742 = ORIENTED_EDGE ( 'NONE', *, *, #20084, .T. ) ;
#2743 = CARTESIAN_POINT ( 'NONE',  ( 157.4999999999998579, 173.6043123611196961, 45.00000000000000000 ) ) ;
#2744 = CARTESIAN_POINT ( 'NONE',  ( 157.4999999999998579, 186.1436873986549188, -45.00000000000000000 ) ) ;
#2745 = LINE ( 'NONE', #18132, #9284 ) ;
#2746 = LINE ( 'NONE', #7067, #18086 ) ;
#2747 = ORIENTED_EDGE ( 'NONE', *, *, #18498, .F. ) ;
#2748 = PLANE ( 'NONE',  #7343 ) ;
#2749 = VECTOR ( 'NONE', #22212, 1000.000000000000000 ) ;
#2750 = ADVANCED_FACE ( 'NONE', ( #676 ), #18614, .F. ) ;
#2751 = CARTESIAN_POINT ( 'NONE',  ( -233.5270925706182084, 66.28764270640111533, 15.64035431904695805 ) ) ;
#2752 = CARTESIAN_POINT ( 'NONE',  ( 157.9999999999996589, 276.1732501651540588, 45.00000000000000000 ) ) ;
#2753 = EDGE_LOOP ( 'NONE', ( #26641, #12361, #6078, #23797 ) ) ;
#2754 = EDGE_LOOP ( 'NONE', ( #2125, #21029, #23401, #26672 ) ) ;
#2755 = AXIS2_PLACEMENT_3D ( 'NONE', #10625, #15513, #6729 ) ;
#2756 = CARTESIAN_POINT ( 'NONE',  ( 158.0000000000011084, 100.6219996396619791, -45.00000000000000000 ) ) ;
#2757 = DIRECTION ( 'NONE',  ( -0.000000000000000000, -0.000000000000000000, -1.000000000000000000 ) ) ;
#2758 = ORIENTED_EDGE ( 'NONE', *, *, #11844, .T. ) ;
#2759 = EDGE_CURVE ( 'NONE', #21594, #12113, #12588, .T. ) ;
#2760 = ORIENTED_EDGE ( 'NONE', *, *, #14624, .F. ) ;
#2761 = ADVANCED_FACE ( 'NONE', ( #10279, #21327 ), #25499, .T. ) ;
#2762 = DIRECTION ( 'NONE',  ( 0.9985600561963485777, -0.05364526231779676024, 0.000000000000000000 ) ) ;
#2763 = EDGE_CURVE ( 'NONE', #9667, #19459, #5816, .T. ) ;
#2764 = CARTESIAN_POINT ( 'NONE',  ( 157.9999999999998010, 238.5551250525490161, 45.00000000000000000 ) ) ;
#2765 = EDGE_CURVE ( 'NONE', #16796, #20071, #12306, .T. ) ;
#2766 = EDGE_LOOP ( 'NONE', ( #16076, #1248, #23199, #17925 ) ) ;
#2767 = CARTESIAN_POINT ( 'NONE',  ( 158.0000000000006253, 146.2716247822957598, -45.00000000000000000 ) ) ;
#2768 = VERTEX_POINT ( 'NONE', #12726 ) ;
#2769 = DIRECTION ( 'NONE',  ( -0.000000000000000000, -0.000000000000000000, -1.000000000000000000 ) ) ;
#2770 = AXIS2_PLACEMENT_3D ( 'NONE', #28338, #15160, #19734 ) ;
#2771 = DIRECTION ( 'NONE',  ( 4.540956701092242152E-16, 1.000000000000000000, 0.000000000000000000 ) ) ;
#2772 = CARTESIAN_POINT ( 'NONE',  ( -68.57415822541635464, -23.01420295945612082, 95.00000000000000000 ) ) ;
#2773 = CARTESIAN_POINT ( 'NONE',  ( -23.72765020131021529, 129.3221281329265366, -15.61619972759512720 ) ) ;
#2774 = CARTESIAN_POINT ( 'NONE',  ( 179.9999999999999147, 494.4107529906318632, 84.99999999999997158 ) ) ;
#2775 = DIRECTION ( 'NONE',  ( -0.8916010070296940260, -0.4528218681376106058, 0.000000000000000000 ) ) ;
#2776 = VECTOR ( 'NONE', #15227, 1000.000000000000000 ) ;
#2777 = CARTESIAN_POINT ( 'NONE',  ( -290.0000000000001137, -157.0000000000000284, 60.00000000000002842 ) ) ;
#2778 = ORIENTED_EDGE ( 'NONE', *, *, #25500, .T. ) ;
#2779 = CARTESIAN_POINT ( 'NONE',  ( 132.3894761555990556, 200.1711027725235397, 45.00000000000000000 ) ) ;
#2780 = DIRECTION ( 'NONE',  ( -0.7071067811865614505, -0.7071067811865336949, 0.000000000000000000 ) ) ;
#2781 = DIRECTION ( 'NONE',  ( 0.4528218681375306698, -0.8916010070297345491, 0.000000000000000000 ) ) ;
#2782 = CARTESIAN_POINT ( 'NONE',  ( 65.00000000000000000, -170.0000000000000853, -69.99999999999998579 ) ) ;
#2783 = EDGE_LOOP ( 'NONE', ( #4645, #20293, #6997, #15217 ) ) ;
#2784 = CARTESIAN_POINT ( 'NONE',  ( -77.29631966220713934, 4.740818392941742232, -13.00000000000000000 ) ) ;
#2785 = ORIENTED_EDGE ( 'NONE', *, *, #10230, .T. ) ;
#2786 = CARTESIAN_POINT ( 'NONE',  ( 157.9999999999997726, 246.0787500750700474, 45.00000000000000000 ) ) ;
#2787 = CARTESIAN_POINT ( 'NONE',  ( 179.9999999999999147, 0.000000000000000000, 100.0000000000000142 ) ) ;
#2788 = CARTESIAN_POINT ( 'NONE',  ( 140.4672727784185327, 249.4977086558912731, -142.5205423047663373 ) ) ;
#2789 = ORIENTED_EDGE ( 'NONE', *, *, #758, .F. ) ;
#2790 = PRESENTATION_STYLE_ASSIGNMENT (( #4653 ) ) ;
#2791 = FILL_AREA_STYLE ('',( #7682 ) ) ;
#2792 = ORIENTED_EDGE ( 'NONE', *, *, #22790, .F. ) ;
#2793 = EDGE_CURVE ( 'NONE', #10017, #14295, #2537, .T. ) ;
#2794 = EDGE_CURVE ( 'NONE', #16382, #12868, #16604, .T. ) ;
#2795 = VECTOR ( 'NONE', #23029, 1000.000000000000000 ) ;
#2796 = CARTESIAN_POINT ( 'NONE',  ( 161.9999999999998863, 220.0000000000000284, -119.9999999999999858 ) ) ;
#2797 = ORIENTED_EDGE ( 'NONE', *, *, #24019, .F. ) ;
#2798 = CARTESIAN_POINT ( 'NONE',  ( -261.1919288306253293, -171.9377729149742038, -104.9999999999998721 ) ) ;
#2799 = VERTEX_POINT ( 'NONE', #19169 ) ;
#2800 = VERTEX_POINT ( 'NONE', #7835 ) ;
#2801 = CARTESIAN_POINT ( 'NONE',  ( 157.9999999999998579, 219.0000000000000284, -45.00000000000000000 ) ) ;
#2802 = VERTEX_POINT ( 'NONE', #1646 ) ;
#2803 = AXIS2_PLACEMENT_3D ( 'NONE', #20977, #25146, #18683 ) ;
#2804 = EDGE_CURVE ( 'NONE', #16689, #13440, #17159, .T. ) ;
#2805 = ORIENTED_EDGE ( 'NONE', *, *, #13521, .F. ) ;
#2806 = ORIENTED_EDGE ( 'NONE', *, *, #28361, .T. ) ;
#2807 = CARTESIAN_POINT ( 'NONE',  ( 95.18208312637723623, 240.6790578601105892, 9.159889466451698325 ) ) ;
#2808 = CARTESIAN_POINT ( 'NONE',  ( -224.0246150495857478, 134.1142769380917343, 12.98324324876687719 ) ) ;
#2809 = DIRECTION ( 'NONE',  ( 0.4528218681376712240, -0.8916010070296632728, 0.000000000000000000 ) ) ;
#2810 = CARTESIAN_POINT ( 'NONE',  ( 157.4999999999998579, 141.0019372635281627, 45.00000000000000000 ) ) ;
#2811 = CARTESIAN_POINT ( 'NONE',  ( 187.4999999999996305, 40.68693696324645970, 45.00000000000000000 ) ) ;
#2812 = DIRECTION ( 'NONE',  ( 0.000000000000000000, 0.000000000000000000, -1.000000000000000000 ) ) ;
#2813 = AXIS2_PLACEMENT_3D ( 'NONE', #28244, #23957, #2106 ) ;
#2814 = DIRECTION ( 'NONE',  ( -0.9659258262890670910, 0.2588190451025251804, 0.000000000000000000 ) ) ;
#2815 = CARTESIAN_POINT ( 'NONE',  ( -272.9143904460767658, -165.1584295805091642, 108.4134862853730965 ) ) ;
#2816 = CARTESIAN_POINT ( 'NONE',  ( 158.0000000000017053, 45.44874947450702507, 45.00000000000000000 ) ) ;
#2817 = PLANE ( 'NONE',  #28111 ) ;
#2818 = VECTOR ( 'NONE', #7258, 1000.000000000000000 ) ;
#2819 = VERTEX_POINT ( 'NONE', #27783 ) ;
#2820 = FACE_OUTER_BOUND ( 'NONE', #14547, .T. ) ;
#2821 = VECTOR ( 'NONE', #7715, 1000.000000000000000 ) ;
#2822 = CARTESIAN_POINT ( 'NONE',  ( -175.8417606860892874, 246.9430296707336652, -15.00000000000000000 ) ) ;
#2823 = LINE ( 'NONE', #11617, #23613 ) ;
#2824 = DIRECTION ( 'NONE',  ( 1.000000000000000000, 0.000000000000000000, 0.000000000000000000 ) ) ;
#2825 = EDGE_LOOP ( 'NONE', ( #22493, #14150, #12355, #13881 ) ) ;
#2826 = EDGE_CURVE ( 'NONE', #8811, #11251, #24124, .T. ) ;
#2827 = CARTESIAN_POINT ( 'NONE',  ( 109.7839892703133984, 255.7665025292603787, -41.33169715142309997 ) ) ;
#2828 = VERTEX_POINT ( 'NONE', #14453 ) ;
#2829 = DIRECTION ( 'NONE',  ( 4.625929269271485914E-16, -1.000000000000000000, 0.000000000000000000 ) ) ;
#2830 = B_SPLINE_CURVE_WITH_KNOTS ( 'NONE', 3,
 ( #15606, #24348, #4662, #13445, #19754, #4381, #12886, #22201, #19618, #26357, #24215, #23935 ),
 .UNSPECIFIED., .F., .F.,
 ( 4, 2, 2, 2, 2, 4 ),
 ( 0.000000000000000000, 0.004258726182425120153, 0.006388089273637603469, 0.008517452364850087651, 0.01277617854727505428, 0.01703490472970001918 ),
 .UNSPECIFIED. ) ;
#2831 = EDGE_LOOP ( 'NONE', ( #442, #8029, #18174, #19658 ) ) ;
#2832 = CIRCLE ( 'NONE', #5586, 5.000000000000004441 ) ;
#2833 = ORIENTED_EDGE ( 'NONE', *, *, #13776, .T. ) ;
#2834 = ORIENTED_EDGE ( 'NONE', *, *, #25622, .T. ) ;
#2835 = VERTEX_POINT ( 'NONE', #3802 ) ;
#2836 = AXIS2_PLACEMENT_3D ( 'NONE', #4769, #6783, #21876 ) ;
#2837 = DIRECTION ( 'NONE',  ( 0.000000000000000000, 0.000000000000000000, -1.000000000000000000 ) ) ;
#2838 = PRODUCT_DEFINITION_FORMATION_WITH_SPECIFIED_SOURCE ( 'ANY', '', #19684, .NOT_KNOWN. ) ;
#2839 = CARTESIAN_POINT ( 'NONE',  ( -175.0000000000000000, -150.0000000000000853, 64.00000000000002842 ) ) ;
#2840 = LINE ( 'NONE', #20225, #20756 ) ;
#2841 = TOROIDAL_SURFACE ( 'NONE', #3301, -538.1631314933625845, 562.1290781602207289 ) ;
#2842 = EDGE_CURVE ( 'NONE', #10961, #11100, #8119, .T. ) ;
#2843 = ADVANCED_FACE ( 'NONE', ( #27915 ), #23630, .F. ) ;
#2844 = CARTESIAN_POINT ( 'NONE',  ( -100.4013316720778874, 135.9145549716820938, -13.58265865227119029 ) ) ;
#2845 = LINE ( 'NONE', #20656, #9838 ) ;
#2846 = DIRECTION ( 'NONE',  ( 1.000000000000000000, 0.000000000000000000, 0.000000000000000000 ) ) ;
#2847 = LINE ( 'NONE', #11639, #4974 ) ;
#2848 = CARTESIAN_POINT ( 'NONE',  ( -113.0191929279866230, 134.5409307879479002, -13.86300596970152377 ) ) ;
#2849 = CARTESIAN_POINT ( 'NONE',  ( 79.99999999999991473, 109.0404994605766831, -77.77847705527373989 ) ) ;
#2850 = CARTESIAN_POINT ( 'NONE',  ( 151.9705627484769650, 235.5563491861038017, 45.00000000000000000 ) ) ;
#2851 = DIRECTION ( 'NONE',  ( -0.000000000000000000, 1.000000000000000000, 0.000000000000000000 ) ) ;
#2852 = DIRECTION ( 'NONE',  ( 1.000000000000000000, -0.000000000000000000, -0.000000000000000000 ) ) ;
#2853 = DIRECTION ( 'NONE',  ( 0.000000000000000000, 0.000000000000000000, -1.000000000000000000 ) ) ;
#2854 = ADVANCED_FACE ( 'NONE', ( #3940 ), #18750, .T. ) ;
#2855 = VECTOR ( 'NONE', #24756, 1000.000000000000114 ) ;
#2856 = EDGE_CURVE ( 'NONE', #16854, #11176, #25917, .T. ) ;
#2857 = CIRCLE ( 'NONE', #5602, 5.000000000000004441 ) ;
#2858 = CARTESIAN_POINT ( 'NONE',  ( 8.117852850209661852, 141.5785587194356481, 14.99999999999999467 ) ) ;
#2859 = DIRECTION ( 'NONE',  ( -0.000000000000000000, -0.000000000000000000, -1.000000000000000000 ) ) ;
#2860 = CARTESIAN_POINT ( 'NONE',  ( -163.8466752748964836, 118.1093140208040069, 24.36087108768327880 ) ) ;
#2861 = CARTESIAN_POINT ( 'NONE',  ( 157.4999999999998295, 218.7460624962465090, 45.00000000000000000 ) ) ;
#2862 = AXIS2_PLACEMENT_3D ( 'NONE', #20346, #22362, #11460 ) ;
#2864 = ORIENTED_EDGE ( 'NONE', *, *, #21490, .F. ) ;
#2863 = ORIENTED_EDGE ( 'NONE', *, *, #27885, .T. ) ;
#2865 = CARTESIAN_POINT ( 'NONE',  ( -205.4480570425783412, 90.78711157365827944, -28.57879582564067533 ) ) ;
#2866 = VECTOR ( 'NONE', #9491, 1000.000000000000000 ) ;
#2867 = CARTESIAN_POINT ( 'NONE',  ( 217.4999999999996305, 258.6181251126050711, 1.387778780781445676E-14 ) ) ;
#2868 = ORIENTED_EDGE ( 'NONE', *, *, #7063, .T. ) ;
#2869 = ORIENTED_EDGE ( 'NONE', *, *, #26398, .T. ) ;
#2870 = ORIENTED_EDGE ( 'NONE', *, *, #14550, .T. ) ;
#2871 = CARTESIAN_POINT ( 'NONE',  ( 157.9999999999996874, 264.1417501351260171, 45.00000000000000000 ) ) ;
#2872 = CARTESIAN_POINT ( 'NONE',  ( -112.9120396111939897, 134.5581283993135173, 15.44207887828286552 ) ) ;
#2873 = VERTEX_POINT ( 'NONE', #10139 ) ;
#2874 = ORIENTED_EDGE ( 'NONE', *, *, #18254, .T. ) ;
#2875 = FACE_OUTER_BOUND ( 'NONE', #25974, .T. ) ;
#2876 = AXIS2_PLACEMENT_3D ( 'NONE', #26536, #1872, #23869 ) ;
#2877 = DIRECTION ( 'NONE',  ( 0.8916010070293584056, -0.4528218681382712996, 0.000000000000000000 ) ) ;
#2878 = ADVANCED_FACE ( 'NONE', ( #19315 ), #28058, .T. ) ;
#2879 = ADVANCED_FACE ( 'NONE', ( #6241 ), #23209, .F. ) ;
#2880 = VECTOR ( 'NONE', #26856, 1000.000000000000114 ) ;
#2881 = CARTESIAN_POINT ( 'NONE',  ( 157.4999999999998579, 88.33656210588026170, 45.00000000000000000 ) ) ;
#2882 = ORIENTED_EDGE ( 'NONE', *, *, #28094, .F. ) ;
#2883 = LINE ( 'NONE', #26579, #15567 ) ;
#2884 = CIRCLE ( 'NONE', #25359, 22.49999999999999289 ) ;
#2885 = CARTESIAN_POINT ( 'NONE',  ( 88.54392521371902092, 230.0000000000000000, -16.22216523460573256 ) ) ;
#2886 = AXIS2_PLACEMENT_3D ( 'NONE', #15750, #13738, #2083 ) ;
#2887 = DIRECTION ( 'NONE',  ( 0.000000000000000000, 0.000000000000000000, -1.000000000000000000 ) ) ;
#2888 = DIRECTION ( 'NONE',  ( 0.4528218681369517995, -0.8916010070300285362, 0.000000000000000000 ) ) ;
#2889 = CARTESIAN_POINT ( 'NONE',  ( -213.2358879321101313, 57.03087831670951147, -38.93822867433466683 ) ) ;
#2890 = EDGE_CURVE ( 'NONE', #24769, #999, #18891, .T. ) ;
#2891 = CARTESIAN_POINT ( 'NONE',  ( -2.862293735361731706E-14, 109.9999999999999858, -70.00000000000001421 ) ) ;
#2892 = DIRECTION ( 'NONE',  ( -0.8916010070295820045, -0.4528218681378310406, 0.000000000000000000 ) ) ;
#2893 = DIRECTION ( 'NONE',  ( -1.000000000000000000, 0.000000000000000000, 0.000000000000000000 ) ) ;
#2894 = PLANE ( 'NONE',  #6162 ) ;
#2895 = ORIENTED_EDGE ( 'NONE', *, *, #8348, .T. ) ;
#2896 = ADVANCED_FACE ( 'NONE', ( #15306 ), #350, .F. ) ;
#2897 = AXIS2_PLACEMENT_3D ( 'NONE', #9814, #27318, #12824 ) ;
#2898 = CARTESIAN_POINT ( 'NONE',  ( 144.9999999999998863, 220.0000000000000284, -99.00000000000001421 ) ) ;
#2899 = EDGE_CURVE ( 'NONE', #9431, #16453, #26057, .T. ) ;
#2900 = AXIS2_PLACEMENT_3D ( 'NONE', #5795, #12279, #19011 ) ;
#2901 = CARTESIAN_POINT ( 'NONE',  ( -236.2188936948037110, 81.35702876104957681, 15.00000000000000000 ) ) ;
#2902 = FACE_OUTER_BOUND ( 'NONE', #28230, .T. ) ;
#2903 = ORIENTED_EDGE ( 'NONE', *, *, #600, .F. ) ;
#2904 = EDGE_CURVE ( 'NONE', #12426, #17375, #26619, .T. ) ;
#2905 = TOROIDAL_SURFACE ( 'NONE', #4718, 19.29759039828519818, 4.355764593064427537 ) ;
#2906 = VERTEX_POINT ( 'NONE', #10703 ) ;
#2907 = CARTESIAN_POINT ( 'NONE',  ( 79.99999999999991473, 110.0000000000000142, 70.00000000000001421 ) ) ;
#2908 = DIRECTION ( 'NONE',  ( -0.000000000000000000, 1.000000000000000000, -1.387778780781445429E-16 ) ) ;
#2909 = ORIENTED_EDGE ( 'NONE', *, *, #14447, .T. ) ;
#2910 = ORIENTED_EDGE ( 'NONE', *, *, #25628, .T. ) ;
#2911 = DIRECTION ( 'NONE',  ( 0.05364526231776645809, -0.9985600561963501320, 0.000000000000000000 ) ) ;
#2912 = CARTESIAN_POINT ( 'NONE',  ( -215.4886702565632106, 139.8420026707765942, 13.00000000000000000 ) ) ;
#2913 = ORIENTED_EDGE ( 'NONE', *, *, #801, .T. ) ;
#2914 = PLANE ( 'NONE',  #24752 ) ;
#2915 = EDGE_LOOP ( 'NONE', ( #12043, #16735, #15307, #27801 ) ) ;
#2916 = TOROIDAL_SURFACE ( 'NONE', #12571, 16.91094714394370158, 6.204828372381208546 ) ;
#2917 = DIRECTION ( 'NONE',  ( 1.000000000000000000, 1.321694076934710155E-16, 0.000000000000000000 ) ) ;
#2918 = AXIS2_PLACEMENT_3D ( 'NONE', #19854, #6923, #2041 ) ;
#2919 = LINE ( 'NONE', #11703, #13120 ) ;
#2920 = CARTESIAN_POINT ( 'NONE',  ( 157.4999999999998010, 238.8090625563025071, -45.00000000000000000 ) ) ;
#2921 = CARTESIAN_POINT ( 'NONE',  ( -24.81898458245972350, 129.2519120894625644, -16.96078301911394703 ) ) ;
#2922 = CIRCLE ( 'NONE', #20808, 2.586968381275096984 ) ;
#2923 = CARTESIAN_POINT ( 'NONE',  ( 164.9999999999998579, 220.0000000000000284, -169.9999999999999716 ) ) ;
#2924 = DIRECTION ( 'NONE',  ( 0.000000000000000000, 0.000000000000000000, 1.000000000000000000 ) ) ;
#2925 = DIRECTION ( 'NONE',  ( -0.000000000000000000, -0.000000000000000000, -1.000000000000000000 ) ) ;
#2926 = ORIENTED_EDGE ( 'NONE', *, *, #20422, .F. ) ;
#2927 = CARTESIAN_POINT ( 'NONE',  ( 46.36636626309694975, -15.13258561588589757, -45.00000000000000000 ) ) ;
#2928 = EDGE_CURVE ( 'NONE', #26764, #20915, #60, .T. ) ;
#2929 = CARTESIAN_POINT ( 'NONE',  ( 139.9999999999999147, -120.0000000000000284, 100.0000000000000142 ) ) ;
#2930 = DIRECTION ( 'NONE',  ( 0.2588190451024993122, -0.9659258262890740854, 0.000000000000000000 ) ) ;
#2931 = LINE ( 'NONE', #25742, #1566 ) ;
#2932 = ORIENTED_EDGE ( 'NONE', *, *, #18092, .T. ) ;
#2933 = LINE ( 'NONE', #11854, #21069 ) ;
#2934 = EDGE_CURVE ( 'NONE', #6860, #23545, #18607, .T. ) ;
#2935 = EDGE_LOOP ( 'NONE', ( #21491, #18936, #1565 ) ) ;
#2936 = EDGE_CURVE ( 'NONE', #7575, #13442, #3014, .T. ) ;
#2937 = CARTESIAN_POINT ( 'NONE',  ( 134.9999999999998579, 220.0000000000000284, 153.1081322850112940 ) ) ;
#2938 = DIRECTION ( 'NONE',  ( 0.000000000000000000, -1.000000000000000000, 0.000000000000000000 ) ) ;
#2939 = VERTEX_POINT ( 'NONE', #15446 ) ;
#2940 = DIRECTION ( 'NONE',  ( -0.000000000000000000, -0.000000000000000000, -1.000000000000000000 ) ) ;
#2941 = CARTESIAN_POINT ( 'NONE',  ( 134.9999999999998579, 220.0000000000000284, 99.00000000000001421 ) ) ;
#2942 = ORIENTED_EDGE ( 'NONE', *, *, #14191, .T. ) ;
#2943 = VECTOR ( 'NONE', #15511, 1000.000000000000000 ) ;
#2944 = CARTESIAN_POINT ( 'NONE',  ( 282.4999999999996589, 19.41075299063184900, 95.49671038392668265 ) ) ;
#2945 = CARTESIAN_POINT ( 'NONE',  ( -277.2150368962633706, -170.0000000000001137, 101.5769467933889558 ) ) ;
#2946 = ORIENTED_EDGE ( 'NONE', *, *, #5275, .T. ) ;
#2947 = AXIS2_PLACEMENT_3D ( 'NONE', #24170, #19708, #32 ) ;
#2948 = VERTEX_POINT ( 'NONE', #4786 ) ;
#2949 = CARTESIAN_POINT ( 'NONE',  ( 157.9999999999998295, 228.5236250225210313, 45.00000000000000000 ) ) ;
#2950 = VERTEX_POINT ( 'NONE', #8548 ) ;
#2951 = VERTEX_POINT ( 'NONE', #24194 ) ;
#2952 = ORIENTED_EDGE ( 'NONE', *, *, #3192, .F. ) ;
#2953 = DIRECTION ( 'NONE',  ( 0.8916010070298968637, 0.4528218681372110366, 0.000000000000000000 ) ) ;
#2954 = CARTESIAN_POINT ( 'NONE',  ( -189.8086322075389774, 92.49158130768422836, -15.00000000000000000 ) ) ;
#2955 = DIRECTION ( 'NONE',  ( 0.8916010070297643031, -0.4528218681374719945, 0.000000000000000000 ) ) ;
#2956 = CIRCLE ( 'NONE', #22235, 10.00000000000000000 ) ;
#2957 = LINE ( 'NONE', #20486, #13333 ) ;
#2958 = CARTESIAN_POINT ( 'NONE',  ( 158.0000000000006537, 143.2558747672816821, 45.00000000000000000 ) ) ;
#2959 = DIRECTION ( 'NONE',  ( -0.000000000000000000, -0.000000000000000000, -1.000000000000000000 ) ) ;
#2960 = DIRECTION ( 'NONE',  ( 0.000000000000000000, 0.000000000000000000, -1.000000000000000000 ) ) ;
#2961 = LINE ( 'NONE', #3094, #258 ) ;
#2962 = AXIS2_PLACEMENT_3D ( 'NONE', #11758, #16063, #7143 ) ;
#2963 = CARTESIAN_POINT ( 'NONE',  ( -261.1919288306253293, -171.9377729149742038, 105.0000000000000142 ) ) ;
#2964 = DIRECTION ( 'NONE',  ( 1.000000000000000000, -0.000000000000000000, -0.000000000000000000 ) ) ;
#2965 = VERTEX_POINT ( 'NONE', #13013 ) ;
#2966 = ADVANCED_FACE ( 'NONE', ( #4494 ), #22036, .F. ) ;
#2967 = ADVANCED_FACE ( 'NONE', ( #11122 ), #19879, .T. ) ;
#2968 = DIRECTION ( 'NONE',  ( -0.000000000000000000, -0.000000000000000000, -1.000000000000000000 ) ) ;
#2969 = CARTESIAN_POINT ( 'NONE',  ( 157.4999999999998579, 48.21056198576756202, -45.00000000000000000 ) ) ;
#2970 = DIRECTION ( 'NONE',  ( -0.000000000000000000, -0.000000000000000000, -1.000000000000000000 ) ) ;
#2971 = ORIENTED_EDGE ( 'NONE', *, *, #602, .F. ) ;
#2972 = DIRECTION ( 'NONE',  ( -1.321694076934710155E-16, 1.000000000000000000, 0.000000000000000000 ) ) ;
#2973 = VERTEX_POINT ( 'NONE', #15730 ) ;
#2974 = CARTESIAN_POINT ( 'NONE',  ( 157.4999999999998579, 161.0649373235845019, 45.00000000000000000 ) ) ;
#2975 = VECTOR ( 'NONE', #26273, 1000.000000000000000 ) ;
#2976 = ORIENTED_EDGE ( 'NONE', *, *, #25059, .T. ) ;
#2977 = VERTEX_POINT ( 'NONE', #17724 ) ;
#2978 = ORIENTED_EDGE ( 'NONE', *, *, #3119, .F. ) ;
#2979 = VECTOR ( 'NONE', #13163, 1000.000000000000000 ) ;
#2980 = ORIENTED_EDGE ( 'NONE', *, *, #16533, .T. ) ;
#2981 = LINE ( 'NONE', #7160, #15959 ) ;
#2982 = DIRECTION ( 'NONE',  ( 0.000000000000000000, 0.000000000000000000, 1.000000000000000000 ) ) ;
#2983 = CARTESIAN_POINT ( 'NONE',  ( 367.9108539694884144, 19.41075299063184900, 87.99671038392668265 ) ) ;
#2984 = CARTESIAN_POINT ( 'NONE',  ( -92.73537453553964838, 136.3631398600097100, -15.17402401083296404 ) ) ;
#2985 = EDGE_CURVE ( 'NONE', #26387, #28088, #26470, .T. ) ;
#2986 = CARTESIAN_POINT ( 'NONE',  ( -42.53273978471831640, 130.9733465240572627, 14.93735646117640847 ) ) ;
#2987 = CARTESIAN_POINT ( 'NONE',  ( -213.9337484054510128, 55.48171494544478577, 43.35284082257812344 ) ) ;
#2988 = DIRECTION ( 'NONE',  ( -0.000000000000000000, -0.000000000000000000, -1.000000000000000000 ) ) ;
#2989 = EDGE_CURVE ( 'NONE', #1063, #15830, #8684, .T. ) ;
#2990 = CARTESIAN_POINT ( 'NONE',  ( -92.74367724329803764, 136.3628496310008131, -13.49999433412610728 ) ) ;
#2991 = CARTESIAN_POINT ( 'NONE',  ( 79.99999999999997158, 103.8532287674466374, -88.29969375664609288 ) ) ;
#2992 = AXIS2_PLACEMENT_3D ( 'NONE', #7090, #26770, #20999 ) ;
#2993 = DIRECTION ( 'NONE',  ( 1.000000000000000000, 0.000000000000000000, -0.000000000000000000 ) ) ;
#2994 = CARTESIAN_POINT ( 'NONE',  ( 157.4999999999998579, 186.1436873986549188, 45.00000000000000000 ) ) ;
#2995 = CARTESIAN_POINT ( 'NONE',  ( 157.9999999999997726, 246.0787500750700474, -45.00000000000000000 ) ) ;
#2996 = DIRECTION ( 'NONE',  ( -0.000000000000000000, -0.000000000000000000, -1.000000000000000000 ) ) ;
#2997 = VECTOR ( 'NONE', #19639, 1000.000000000000000 ) ;
#2998 = EDGE_CURVE ( 'NONE', #23714, #1235, #14208, .T. ) ;
#2999 = CARTESIAN_POINT ( 'NONE',  ( -200.0643534088114848, 95.37219532206381700, 31.11168591751386714 ) ) ;
#3000 = CARTESIAN_POINT ( 'NONE',  ( 125.3433571860710600, 197.9412384757604570, -84.99999999999997158 ) ) ;
#3001 = CIRCLE ( 'NONE', #20434, 5.000000000000004441 ) ;
#3003 = ORIENTED_EDGE ( 'NONE', *, *, #16317, .T. ) ;
#3002 = ORIENTED_EDGE ( 'NONE', *, *, #21641, .F. ) ;
#3004 = CARTESIAN_POINT ( 'NONE',  ( -160.0000000000000568, 230.0000000000000000, 5.000000000000002665 ) ) ;
#3005 = EDGE_CURVE ( 'NONE', #27691, #16717, #15580, .T. ) ;
#3006 = ORIENTED_EDGE ( 'NONE', *, *, #13984, .F. ) ;
#3007 = EDGE_LOOP ( 'NONE', ( #25067, #14646, #11977, #22024 ) ) ;
#3008 = CARTESIAN_POINT ( 'NONE',  ( 158.0000000000004547, 165.8267498348450886, 45.00000000000000000 ) ) ;
#3009 = CARTESIAN_POINT ( 'NONE',  ( -52.56693897510013613, 133.2842826589903495, 15.71165752789189440 ) ) ;
#3010 = ORIENTED_EDGE ( 'NONE', *, *, #6883, .F. ) ;
#3011 = AXIS2_PLACEMENT_3D ( 'NONE', #23167, #8076, #5915 ) ;
#3012 = VERTEX_POINT ( 'NONE', #4639 ) ;
#3013 = DIRECTION ( 'NONE',  ( 0.4528218681371123377, 0.8916010070299471568, -0.000000000000000000 ) ) ;
#3014 = CIRCLE ( 'NONE', #9898, 75.00000000000002842 ) ;
#3015 = VECTOR ( 'NONE', #6084, 1000.000000000000000 ) ;
#3016 = EDGE_CURVE ( 'NONE', #9494, #17780, #13574, .T. ) ;
#3017 = CARTESIAN_POINT ( 'NONE',  ( 267.4999999999996021, 194.4107529906318064, 75.35061095560300259 ) ) ;
#3018 = CARTESIAN_POINT ( 'NONE',  ( 179.9999999999999147, 526.4263741777961059, 84.99999999999997158 ) ) ;
#3019 = AXIS2_PLACEMENT_3D ( 'NONE', #5917, #23445, #1607 ) ;
#3020 = CARTESIAN_POINT ( 'NONE',  ( -260.0000000000001137, -167.0819201924624906, 105.0000000000000142 ) ) ;
#3021 = EDGE_CURVE ( 'NONE', #21473, #465, #15162, .T. ) ;
#3022 = CARTESIAN_POINT ( 'NONE',  ( -175.0000000000000000, -120.0000000000001705, 63.97500000000001563 ) ) ;
#3023 = FACE_OUTER_BOUND ( 'NONE', #17893, .T. ) ;
#3024 = CARTESIAN_POINT ( 'NONE',  ( -203.1048999767863563, 60.64878749907617816, -23.79654850876571359 ) ) ;
#3025 = LINE ( 'NONE', #11815, #5441 ) ;
#3026 = CARTESIAN_POINT ( 'NONE',  ( 3.469446951953618133E-15, -40.00000000000003553, 70.00000000000001421 ) ) ;
#3027 = CARTESIAN_POINT ( 'NONE',  ( -160.0000000000000284, 109.9999999999999432, -45.00000000000000000 ) ) ;
#3028 = FACE_OUTER_BOUND ( 'NONE', #17339, .T. ) ;
#3029 = EDGE_LOOP ( 'NONE', ( #17346, #1832, #6012, #8093 ) ) ;
#3030 = VECTOR ( 'NONE', #28227, 1000.000000000000000 ) ;
#3031 = CARTESIAN_POINT ( 'NONE',  ( 157.9999999999998579, 223.5078750075070104, -45.00000000000000000 ) ) ;
#3032 = EDGE_CURVE ( 'NONE', #212, #5309, #5919, .T. ) ;
#3033 = CARTESIAN_POINT ( 'NONE',  ( -231.9024517383455475, 76.40908368391228578, 15.65418338381032193 ) ) ;
#3034 = DIRECTION ( 'NONE',  ( -0.000000000000000000, -1.000000000000000000, -0.000000000000000000 ) ) ;
#3035 = ORIENTED_EDGE ( 'NONE', *, *, #2045, .F. ) ;
#3036 = AXIS2_PLACEMENT_3D ( 'NONE', #20911, #5961, #12167 ) ;
#3037 = ORIENTED_EDGE ( 'NONE', *, *, #1009, .T. ) ;
#3038 =( REPRESENTATION_RELATIONSHIP ('NONE','NONE', #11963, #14145 ) REPRESENTATION_RELATIONSHIP_WITH_TRANSFORMATION ( #7333 )SHAPE_REPRESENTATION_RELATIONSHIP( ) );
#3039 = DIRECTION ( 'NONE',  ( 0.000000000000000000, 0.000000000000000000, -1.000000000000000000 ) ) ;
#3040 = CARTESIAN_POINT ( 'NONE',  ( -63.57415822541634043, 24.64876300893806160, 100.0000000000000000 ) ) ;
#3041 = VERTEX_POINT ( 'NONE', #10841 ) ;
#3043 = ADVANCED_FACE ( 'NONE', ( #493 ), #22324, .F. ) ;
#3042 = ORIENTED_EDGE ( 'NONE', *, *, #23294, .T. ) ;
#3044 = DIRECTION ( 'NONE',  ( 1.000000000000000000, 0.000000000000000000, 0.000000000000000000 ) ) ;
#3045 = DIRECTION ( 'NONE',  ( 0.000000000000000000, -0.000000000000000000, -1.000000000000000000 ) ) ;
#3046 = PLANE ( 'NONE',  #15104 ) ;
#3047 = ORIENTED_EDGE ( 'NONE', *, *, #13106, .T. ) ;
#3048 = CARTESIAN_POINT ( 'NONE',  ( 0.000000000000000000, 0.000000000000000000, 95.00000000000000000 ) ) ;
#3049 = EDGE_LOOP ( 'NONE', ( #7544, #24574, #24216, #1672 ) ) ;
#3050 = AXIS2_PLACEMENT_3D ( 'NONE', #6788, #8671, #15569 ) ;
#3051 = CARTESIAN_POINT ( 'NONE',  ( 158.0000000000002842, 180.8739998798873501, 45.00000000000000000 ) ) ;
#3052 = EDGE_CURVE ( 'NONE', #24120, #16717, #26777, .T. ) ;
#3053 = LINE ( 'NONE', #9103, #18156 ) ;
#3054 = ADVANCED_FACE ( 'NONE', ( #5361 ), #16433, .F. ) ;
#3055 = CARTESIAN_POINT ( 'NONE',  ( 338.9795809418241106, 102.2323340340494298, -162.9307281190808681 ) ) ;
#3056 = CARTESIAN_POINT ( 'NONE',  ( -23.16458623837309716, 129.3662862396423350, -15.59652033367907364 ) ) ;
#3057 = PLANE ( 'NONE',  #11894 ) ;
#3058 = CARTESIAN_POINT ( 'NONE',  ( 157.4999999999997158, 258.8720626163585621, 45.00000000000000000 ) ) ;
#3059 = CARTESIAN_POINT ( 'NONE',  ( 161.3653042226020204, 205.6814106928004833, -139.0380470571626574 ) ) ;
#3060 = ORIENTED_EDGE ( 'NONE', *, *, #8204, .F. ) ;
#3061 = DIRECTION ( 'NONE',  ( 0.4528218681383106015, -0.8916010070293384215, 0.000000000000000000 ) ) ;
#3062 = LINE ( 'NONE', #25054, #4201 ) ;
#3063 = DIRECTION ( 'NONE',  ( -0.4999999999999985012, -0.8660254037844394848, 0.000000000000000000 ) ) ;
#3064 = EDGE_LOOP ( 'NONE', ( #24679, #9834, #9074, #1280 ) ) ;
#3065 = CARTESIAN_POINT ( 'NONE',  ( 217.4999999999996305, 194.4107529906318064, -100.0000000000000000 ) ) ;
#3066 = ORIENTED_EDGE ( 'NONE', *, *, #8083, .T. ) ;
#3067 = CARTESIAN_POINT ( 'NONE',  ( 158.0000000000007105, 136.2401247522676044, 45.00000000000000000 ) ) ;
#3068 = PLANE ( 'NONE',  #5509 ) ;
#3069 = CARTESIAN_POINT ( 'NONE',  ( -231.9378824387731299, 93.53122965655670384, 12.99999999999999822 ) ) ;
#3070 = ORIENTED_EDGE ( 'NONE', *, *, #1754, .F. ) ;
#3071 = CARTESIAN_POINT ( 'NONE',  ( -42.99650729631200363, 71.03850157808263077, 99.00000000000000000 ) ) ;
#3072 = EDGE_LOOP ( 'NONE', ( #18178, #16627, #23320, #26522 ) ) ;
#3073 = VECTOR ( 'NONE', #26874, 1000.000000000000000 ) ;
#3074 = CIRCLE ( 'NONE', #9512, 2.586968381275096984 ) ;
#3075 = CYLINDRICAL_SURFACE ( 'NONE', #18500, 19.99999999999998934 ) ;
#3076 = CARTESIAN_POINT ( 'NONE',  ( 100.4596905818591921, 242.9371963736508917, 14.31527322455832518 ) ) ;
#3077 = ORIENTED_EDGE ( 'NONE', *, *, #26807, .F. ) ;
#3078 = ORIENTED_EDGE ( 'NONE', *, *, #1620, .F. ) ;
#3079 = LINE ( 'NONE', #16039, #11336 ) ;
#3080 = ORIENTED_EDGE ( 'NONE', *, *, #12830, .T. ) ;
#3081 = VERTEX_POINT ( 'NONE', #9253 ) ;
#3082 = EDGE_LOOP ( 'NONE', ( #22866, #18073, #13925, #14229, #8531, #24826, #24828, #23547, #2946, #19715, #21670 ) ) ;
#3083 = ADVANCED_FACE ( 'NONE', ( #15877 ), #25050, .F. ) ;
#3084 = DIRECTION ( 'NONE',  ( 0.4528218681375507093, -0.8916010070297244461, 0.000000000000000000 ) ) ;
#3085 = EDGE_CURVE ( 'NONE', #24784, #22271, #7388, .T. ) ;
#3086 = DIRECTION ( 'NONE',  ( -0.8916010070291696676, -0.4528218681386429467, 0.000000000000000000 ) ) ;
#3087 = CARTESIAN_POINT ( 'NONE',  ( 157.9999999999998010, 234.0472500450420341, 45.00000000000000000 ) ) ;
#3088 = CIRCLE ( 'NONE', #356, 10.00000000000000888 ) ;
#3089 = AXIS2_PLACEMENT_3D ( 'NONE', #11013, #1951, #28231 ) ;
#3090 = CARTESIAN_POINT ( 'NONE',  ( 96.92716526682083611, 115.1868982021453149, -77.49999999976235188 ) ) ;
#3091 = CARTESIAN_POINT ( 'NONE',  ( 193.7634559672933676, 193.7634559672857790, 45.00000000000000000 ) ) ;
#3092 = CARTESIAN_POINT ( 'NONE',  ( -26.23654403271235225, 26.23654403271337543, 45.00000000000000000 ) ) ;
#3093 = CARTESIAN_POINT ( 'NONE',  ( 125.3433571860711453, 242.0587615242396566, 0.000000000000000000 ) ) ;
#3094 = CARTESIAN_POINT ( 'NONE',  ( 158.0000000000005400, 153.7952498048169048, 45.00000000000000000 ) ) ;
#3095 = CARTESIAN_POINT ( 'NONE',  ( -268.7660490202469532, -170.5116556248577524, 109.2537565056162379 ) ) ;
#3096 = DIRECTION ( 'NONE',  ( 0.000000000000000000, 0.000000000000000000, -1.000000000000000000 ) ) ;
#3097 = CARTESIAN_POINT ( 'NONE',  ( 114.1093725872594575, 211.6289295222773603, -98.08429852854942510 ) ) ;
#3098 = ORIENTED_EDGE ( 'NONE', *, *, #12175, .F. ) ;
#3099 = CARTESIAN_POINT ( 'NONE',  ( 158.0000000000012221, 88.59049960963380954, 45.00000000000000000 ) ) ;
#3100 = CARTESIAN_POINT ( 'NONE',  ( 158.0000000000015064, 61.00387452705632541, 45.00000000000000000 ) ) ;
#3101 = DIRECTION ( 'NONE',  ( -0.000000000000000000, 1.000000000000000000, -1.387778780781445429E-16 ) ) ;
#3102 = ORIENTED_EDGE ( 'NONE', *, *, #25457, .T. ) ;
#3103 = AXIS2_PLACEMENT_3D ( 'NONE', #28274, #8473, #17230 ) ;
#3104 = PLANE ( 'NONE',  #24460 ) ;
#3105 = VERTEX_POINT ( 'NONE', #16015 ) ;
#3106 = EDGE_CURVE ( 'NONE', #24374, #14709, #11566, .T. ) ;
#3107 = CARTESIAN_POINT ( 'NONE',  ( 157.4999999999998579, 110.9074371734436255, 45.00000000000000000 ) ) ;
#3108 = EDGE_LOOP ( 'NONE', ( #23647, #22673, #22631, #22062 ) ) ;
#3109 = ORIENTED_EDGE ( 'NONE', *, *, #22979, .F. ) ;
#3110 = ORIENTED_EDGE ( 'NONE', *, *, #9960, .F. ) ;
#3111 = EDGE_CURVE ( 'NONE', #17042, #24468, #21512, .T. ) ;
#3112 = ORIENTED_EDGE ( 'NONE', *, *, #27376, .T. ) ;
#3113 = CARTESIAN_POINT ( 'NONE',  ( -127.8827038603104143, 131.6591692175807964, 14.66642017785206598 ) ) ;
#3114 = FACE_OUTER_BOUND ( 'NONE', #9055, .T. ) ;
#3115 = DIRECTION ( 'NONE',  ( 0.000000000000000000, 0.000000000000000000, 1.000000000000000000 ) ) ;
#3116 = EDGE_CURVE ( 'NONE', #12076, #20506, #14007, .T. ) ;
#3117 = EDGE_CURVE ( 'NONE', #15076, #1070, #10707, .T. ) ;
#3118 = COLOUR_RGB ( '',0.7921568627450980005, 0.8196078431372548767, 0.9333333333333333481 ) ;
#3119 = EDGE_CURVE ( 'NONE', #26387, #27071, #27326, .T. ) ;
#3120 = CARTESIAN_POINT ( 'NONE',  ( -90.19822669564636897, 136.4341346054573876, -15.16547208303790484 ) ) ;
#3121 = CARTESIAN_POINT ( 'NONE',  ( 157.4999999999998579, 220.0000000000000284, 84.99999999999995737 ) ) ;
#3122 = CARTESIAN_POINT ( 'NONE',  ( 338.9795809418241106, 102.2323340340494155, -127.0692718809191035 ) ) ;
#3124 = DIRECTION ( 'NONE',  ( -0.000000000000000000, 1.000000000000000000, 0.000000000000000000 ) ) ;
#3123 = VECTOR ( 'NONE', #22798, 1000.000000000000000 ) ;
#3125 = CARTESIAN_POINT ( 'NONE',  ( -100.3939829605125880, 135.9151291309332521, -13.58254898561143342 ) ) ;
#3126 = PLANE ( 'NONE',  #12679 ) ;
#3127 = LINE ( 'NONE', #13942, #692 ) ;
#3128 = SHAPE_REPRESENTATION ( 'Handel High-Force Electromagnet Base Block', ( #10637 ), #6979 ) ;
#3129 = CARTESIAN_POINT ( 'NONE',  ( 330.9869376377542949, 44.41075299063183479, 288.0938197134494203 ) ) ;
#3130 = CARTESIAN_POINT ( 'NONE',  ( 134.9999999999998579, -327.2004514666934369, -84.99999999999997158 ) ) ;
#3131 = CARTESIAN_POINT ( 'NONE',  ( 209.9999999999999432, -280.0000000000000000, 110.0000000000000284 ) ) ;
#3132 = DIRECTION ( 'NONE',  ( 0.000000000000000000, -0.000000000000000000, 1.000000000000000000 ) ) ;
#3133 = DIRECTION ( 'NONE',  ( 0.000000000000000000, -0.000000000000000000, -1.000000000000000000 ) ) ;
#3134 = CARTESIAN_POINT ( 'NONE',  ( 158.0000000000014779, 65.51174953456337846, 45.00000000000000000 ) ) ;
#3136 = ORIENTED_EDGE ( 'NONE', *, *, #25118, .F. ) ;
#3135 = ORIENTED_EDGE ( 'NONE', *, *, #21874, .T. ) ;
#3137 = AXIS2_PLACEMENT_3D ( 'NONE', #1516, #23639, #8272 ) ;
#3138 = DIRECTION ( 'NONE',  ( -0.9985600561963485777, -0.05364526231779759985, 0.000000000000000000 ) ) ;
#3139 = EDGE_LOOP ( 'NONE', ( #20259, #24153, #27974, #18916 ) ) ;
#3140 = ORIENTED_EDGE ( 'NONE', *, *, #25473, .T. ) ;
#3141 = EDGE_CURVE ( 'NONE', #25239, #18389, #20454, .T. ) ;
#3142 = AXIS2_PLACEMENT_3D ( 'NONE', #11715, #22040, #15736 ) ;
#3143 = EDGE_CURVE ( 'NONE', #14018, #27164, #13719, .T. ) ;
#3144 = DIRECTION ( 'NONE',  ( 0.000000000000000000, 0.000000000000000000, 1.000000000000000000 ) ) ;
#3145 = EDGE_CURVE ( 'NONE', #19755, #3920, #20727, .T. ) ;
#3146 = CIRCLE ( 'NONE', #6824, 6.000000000000005329 ) ;
#3147 = VERTEX_POINT ( 'NONE', #2777 ) ;
#3148 = ORIENTED_EDGE ( 'NONE', *, *, #2429, .T. ) ;
#3149 = CARTESIAN_POINT ( 'NONE',  ( -175.0000000000000000, -150.0000000000000853, -75.99999999999998579 ) ) ;
#3150 = CARTESIAN_POINT ( 'NONE',  ( 157.4999999999998579, 113.4153121809506786, 45.00000000000000000 ) ) ;
#3151 = VECTOR ( 'NONE', #3185, 1000.000000000000000 ) ;
#3152 = EDGE_CURVE ( 'NONE', #11439, #7854, #6559, .T. ) ;
#3153 = CARTESIAN_POINT ( 'NONE',  ( 157.4999999999996589, 273.9193126614005678, 45.00000000000000000 ) ) ;
#3154 = CARTESIAN_POINT ( 'NONE',  ( 92.44908716912959790, 230.7276285284523567, -17.70004843202667644 ) ) ;
#3155 = EDGE_CURVE ( 'NONE', #17557, #4843, #5663, .T. ) ;
#3156 = VECTOR ( 'NONE', #20598, 1000.000000000000000 ) ;
#3157 = VECTOR ( 'NONE', #2121, 1000.000000000000114 ) ;
#3158 = PLANE ( 'NONE',  #5725 ) ;
#3159 = DIRECTION ( 'NONE',  ( -0.000000000000000000, 1.000000000000000000, -1.387778780781445429E-16 ) ) ;
#3160 = CARTESIAN_POINT ( 'NONE',  ( -219.3331038875180639, 71.26739478977619058, -22.27060053768705217 ) ) ;
#3161 = AXIS2_PLACEMENT_3D ( 'NONE', #6603, #4723, #24270 ) ;
#3162 = DIRECTION ( 'NONE',  ( 0.4528218681383106015, -0.8916010070293384215, 0.000000000000000000 ) ) ;
#3163 = CARTESIAN_POINT ( 'NONE',  ( -200.0000000000000284, -120.0000000000001279, -25.00000000000000000 ) ) ;
#3164 = CARTESIAN_POINT ( 'NONE',  ( 145.9999999999998863, 220.0000000000000284, -99.00000000000001421 ) ) ;
#3165 = DIRECTION ( 'NONE',  ( -1.000000000000000000, 0.000000000000000000, -0.000000000000000000 ) ) ;
#3166 = ORIENTED_EDGE ( 'NONE', *, *, #9750, .T. ) ;
#3167 = LINE ( 'NONE', #9656, #23842 ) ;
#3168 = CIRCLE ( 'NONE', #12828, 30.00000000000000000 ) ;
#3169 = CARTESIAN_POINT ( 'NONE',  ( -229.6735579984113258, 64.27833679895920227, 7.258985754582258032 ) ) ;
#3170 = LINE ( 'NONE', #11822, #9439 ) ;
#3171 = ORIENTED_EDGE ( 'NONE', *, *, #23218, .F. ) ;
#3172 = DIRECTION ( 'NONE',  ( 1.000000000000000000, 0.000000000000000000, 0.000000000000000000 ) ) ;
#3173 = ORIENTED_EDGE ( 'NONE', *, *, #15521, .T. ) ;
#3174 = EDGE_CURVE ( 'NONE', #5095, #17304, #27603, .T. ) ;
#3175 = EDGE_CURVE ( 'NONE', #27514, #5337, #19000, .T. ) ;
#3176 = CARTESIAN_POINT ( 'NONE',  ( 98.15430812615089451, 116.0637945823775112, 78.75000000031268144 ) ) ;
#3177 = VECTOR ( 'NONE', #21120, 1000.000000000000114 ) ;
#3178 = DIRECTION ( 'NONE',  ( 0.000000000000000000, -1.000000000000000000, 0.000000000000000000 ) ) ;
#3179 = ORIENTED_EDGE ( 'NONE', *, *, #22787, .F. ) ;
#3180 = VECTOR ( 'NONE', #10372, 1000.000000000000000 ) ;
#3181 = ORIENTED_EDGE ( 'NONE', *, *, #8775, .T. ) ;
#3182 = FACE_OUTER_BOUND ( 'NONE', #20955, .T. ) ;
#3183 = AXIS2_PLACEMENT_3D ( 'NONE', #17308, #4510, #8559 ) ;
#3184 = CARTESIAN_POINT ( 'NONE',  ( 158.0000000000007958, 130.7164997297464595, 45.00000000000000000 ) ) ;
#3185 = DIRECTION ( 'NONE',  ( -0.000000000000000000, -0.000000000000000000, 1.000000000000000000 ) ) ;
#3186 = ORIENTED_EDGE ( 'NONE', *, *, #27187, .T. ) ;
#3187 = DIRECTION ( 'NONE',  ( 1.850371707708594316E-16, -1.000000000000000000, 0.000000000000000000 ) ) ;
#3188 = ORIENTED_EDGE ( 'NONE', *, *, #11568, .T. ) ;
#3189 = CARTESIAN_POINT ( 'NONE',  ( -266.5839533485339530, -91.18033988749901653, 15.26911010665567225 ) ) ;
#3190 = AXIS2_PLACEMENT_3D ( 'NONE', #11487, #8749, #20229 ) ;
#3191 = EDGE_CURVE ( 'NONE', #25446, #25995, #13931, .T. ) ;
#3192 = EDGE_CURVE ( 'NONE', #17930, #19026, #5511, .T. ) ;
#3193 = DIRECTION ( 'NONE',  ( 1.000000000000000000, 2.602085213965211135E-16, -0.000000000000000000 ) ) ;
#3194 = LINE ( 'NONE', #7663, #13532 ) ;
#3195 = LINE ( 'NONE', #27877, #14968 ) ;
#3196 = DIRECTION ( 'NONE',  ( -0.000000000000000000, -0.000000000000000000, -1.000000000000000000 ) ) ;
#3197 = DIRECTION ( 'NONE',  ( -0.000000000000000000, -0.000000000000000000, -1.000000000000000000 ) ) ;
#3198 = CARTESIAN_POINT ( 'NONE',  ( 157.9999999999996589, 271.6653751576470768, 45.00000000000000000 ) ) ;
#3199 = ORIENTED_EDGE ( 'NONE', *, *, #28136, .F. ) ;
#3200 = VECTOR ( 'NONE', #7699, 1000.000000000000000 ) ;
#3201 = FACE_OUTER_BOUND ( 'NONE', #15790, .T. ) ;
#3202 = CARTESIAN_POINT ( 'NONE',  ( 157.9999999999997158, 261.6338751276190351, 45.00000000000000000 ) ) ;
#3203 = FACE_OUTER_BOUND ( 'NONE', #3895, .T. ) ;
#3204 = ORIENTED_EDGE ( 'NONE', *, *, #23367, .T. ) ;
#3205 = EDGE_CURVE ( 'NONE', #11076, #15637, #18257, .T. ) ;
#3206 = LINE ( 'NONE', #25188, #27014 ) ;
#3207 = VECTOR ( 'NONE', #22991, 1000.000000000000000 ) ;
#3208 = ORIENTED_EDGE ( 'NONE', *, *, #15670, .F. ) ;
#3209 = EDGE_CURVE ( 'NONE', #7922, #6186, #22844, .T. ) ;
#3210 = DIRECTION ( 'NONE',  ( -1.000000000000000000, 0.000000000000000000, 0.000000000000000000 ) ) ;
#3211 = FACE_OUTER_BOUND ( 'NONE', #6243, .T. ) ;
#3212 = CARTESIAN_POINT ( 'NONE',  ( 135.9832230577667360, 249.9845044293635965, -139.0778438077165333 ) ) ;
#3213 = ORIENTED_EDGE ( 'NONE', *, *, #16118, .F. ) ;
#3214 = CARTESIAN_POINT ( 'NONE',  ( 157.4999999999997726, 248.8405625863305204, 45.00000000000000000 ) ) ;
#3215 = CARTESIAN_POINT ( 'NONE',  ( 367.4999999999996021, 44.41075299063184900, 1.850330238640837654E-14 ) ) ;
#3216 = ORIENTED_EDGE ( 'NONE', *, *, #8413, .T. ) ;
#3217 = CARTESIAN_POINT ( 'NONE',  ( -85.18883433891745938, 134.8019439274000604, 15.45375652165002656 ) ) ;
#3218 = CARTESIAN_POINT ( 'NONE',  ( -160.0000000000000284, 119.7660240611718621, -22.85081902853005431 ) ) ;
#3219 = ORIENTED_EDGE ( 'NONE', *, *, #9095, .F. ) ;
#3220 = ORIENTED_EDGE ( 'NONE', *, *, #8000, .T. ) ;
#3221 = DIRECTION ( 'NONE',  ( 0.8916010070295511403, -0.4528218681378915478, 0.000000000000000000 ) ) ;
#3222 = VERTEX_POINT ( 'NONE', #20681 ) ;
#3223 = VECTOR ( 'NONE', #11605, 1000.000000000000000 ) ;
#3224 = VERTEX_POINT ( 'NONE', #591 ) ;
#3225 = VERTEX_POINT ( 'NONE', #3149 ) ;
#3226 = CARTESIAN_POINT ( 'NONE',  ( 108.4669391321881591, 252.2354088787809303, 31.48703123558444616 ) ) ;
#3227 = VECTOR ( 'NONE', #9449, 1000.000000000000000 ) ;
#3228 = EDGE_CURVE ( 'NONE', #13771, #11671, #5962, .T. ) ;
#3229 = CARTESIAN_POINT ( 'NONE',  ( -175.0000000000000000, -150.0000000000000853, 76.00000000000001421 ) ) ;
#3230 = B_SPLINE_CURVE_WITH_KNOTS ( 'NONE', 3,
 ( #15011, #21601, #4778, #17430, #8956, #26190, #2477, #22459, #11264, #15721, #6515, #15574, #18009, #19592, #2191, #4486, #19728, #22317, #24052, #2623, #484, #10975 ),
 .UNSPECIFIED., .F., .F.,
 ( 4, 2, 2, 2, 2, 2, 2, 2, 2, 2, 4 ),
 ( 0.000000000000000000, 0.006858469009249849001, 0.01371693801849969800, 0.01714617252312462120, 0.02057540702774954613, 0.02743387603699941335, 0.03429234504624928404, 0.03772157955087421938, 0.04115081405549916860, 0.04800928306474905316, 0.05486775207399893772 ),
 .UNSPECIFIED. ) ;
#3231 = DIRECTION ( 'NONE',  ( 0.4528218681386429467, -0.8916010070291696676, 0.000000000000000000 ) ) ;
#3232 = LINE ( 'NONE', #11747, #9676 ) ;
#3233 = CARTESIAN_POINT ( 'NONE',  ( 157.9999999999996305, 286.7126252026890256, 45.00000000000000000 ) ) ;
#3234 = LINE ( 'NONE', #12020, #3321 ) ;
#3235 = DIRECTION ( 'NONE',  ( -0.8916010070293584056, -0.4528218681382712996, 0.000000000000000000 ) ) ;
#3236 = CARTESIAN_POINT ( 'NONE',  ( -264.2078319525319898, -171.2518620402580325, 109.8556748947001296 ) ) ;
#3237 = CARTESIAN_POINT ( 'NONE',  ( 157.4999999999996589, 278.9350626764145318, 45.00000000000000000 ) ) ;
#3238 = CARTESIAN_POINT ( 'NONE',  ( -76.25760768171835480, 219.6666220619077876, -13.00000000000000000 ) ) ;
#3239 = VERTEX_POINT ( 'NONE', #18396 ) ;
#3240 = MECHANICAL_DESIGN_GEOMETRIC_PRESENTATION_REPRESENTATION (  '', ( #4160 ), #14743 ) ;
#3241 = DIRECTION ( 'NONE',  ( -1.000000000000000000, 0.000000000000000000, 0.000000000000000000 ) ) ;
#3242 = LINE ( 'NONE', #18765, #15841 ) ;
#3243 = DIRECTION ( 'NONE',  ( 0.000000000000000000, 0.000000000000000000, -1.000000000000000000 ) ) ;
#3244 = LINE ( 'NONE', #11619, #15224 ) ;
#3245 = ORIENTED_EDGE ( 'NONE', *, *, #6358, .T. ) ;
#3246 = ADVANCED_FACE ( 'NONE', ( #5597 ), #27148, .F. ) ;
#3247 = ADVANCED_FACE ( 'NONE', ( #5176 ), #22568, .F. ) ;
#3248 = CARTESIAN_POINT ( 'NONE',  ( -260.0000000000001137, -167.0819201924624906, -94.99999999999987210 ) ) ;
#3249 = ORIENTED_EDGE ( 'NONE', *, *, #14777, .T. ) ;
#3250 = FACE_OUTER_BOUND ( 'NONE', #15423, .T. ) ;
#3251 = EDGE_CURVE ( 'NONE', #14501, #26726, #3290, .T. ) ;
#3252 = VERTEX_POINT ( 'NONE', #16254 ) ;
#3253 = ORIENTED_EDGE ( 'NONE', *, *, #19725, .T. ) ;
#3254 = VERTEX_POINT ( 'NONE', #24721 ) ;
#3255 = ORIENTED_EDGE ( 'NONE', *, *, #6714, .F. ) ;
#3256 = DIRECTION ( 'NONE',  ( -0.000000000000000000, -0.000000000000000000, 1.000000000000000000 ) ) ;
#3257 = DIRECTION ( 'NONE',  ( -0.8916010070296632728, 0.4528218681376712240, 0.000000000000000000 ) ) ;
#3258 = DIRECTION ( 'NONE',  ( 0.4528218681382713551, 0.8916010070293584056, -0.000000000000000000 ) ) ;
#3259 = AXIS2_PLACEMENT_3D ( 'NONE', #14736, #14885, #19318 ) ;
#3260 = CARTESIAN_POINT ( 'NONE',  ( -67.51396541345637559, 135.5198389557239693, -15.28949482634511092 ) ) ;
#3261 = CARTESIAN_POINT ( 'NONE',  ( -4.279947336434443805, 134.1643719796016683, 13.92784264465264776 ) ) ;
#3262 = AXIS2_PLACEMENT_3D ( 'NONE', #21260, #14812, #17096 ) ;
#3263 = LINE ( 'NONE', #9888, #1546 ) ;
#3264 = CARTESIAN_POINT ( 'NONE',  ( 185.9255560592262100, 121.0883471088020116, 45.00000000000000000 ) ) ;
#3265 = DIRECTION ( 'NONE',  ( 0.8916010070297446521, 0.4528218681375106858, 0.000000000000000000 ) ) ;
#3266 = CARTESIAN_POINT ( 'NONE',  ( 158.0000000000000284, 203.9527499549551806, -45.00000000000000000 ) ) ;
#3267 = CARTESIAN_POINT ( 'NONE',  ( -217.1524024359874545, 87.79586245209446815, -18.07482474875216738 ) ) ;
#3268 = DIRECTION ( 'NONE',  ( -0.000000000000000000, -0.000000000000000000, -1.000000000000000000 ) ) ;
#3269 = CARTESIAN_POINT ( 'NONE',  ( 157.4999999999998579, 186.1436873986549188, 45.00000000000000000 ) ) ;
#3270 = DIRECTION ( 'NONE',  ( 0.000000000000000000, 0.000000000000000000, 1.000000000000000000 ) ) ;
#3271 = ORIENTED_EDGE ( 'NONE', *, *, #14791, .T. ) ;
#3272 = DIRECTION ( 'NONE',  ( 0.3825563754725206378, 0.000000000000000000, 0.9239321509641971186 ) ) ;
#3273 = CARTESIAN_POINT ( 'NONE',  ( 119.9999999987673220, 136.1131920016294714, -100.0000000000000142 ) ) ;
#3274 = ADVANCED_FACE ( 'NONE', ( #2875 ), #11668, .F. ) ;
#3275 = CARTESIAN_POINT ( 'NONE',  ( -266.5839533485339530, -91.18033988749901653, 0.000000000000000000 ) ) ;
#3277 = EDGE_LOOP ( 'NONE', ( #10786, #8996, #69, #22975 ) ) ;
#3276 = ORIENTED_EDGE ( 'NONE', *, *, #4426, .F. ) ;
#3278 = EDGE_CURVE ( 'NONE', #7087, #17712, #9918, .T. ) ;
#3279 = AXIS2_PLACEMENT_3D ( 'NONE', #8516, #21866, #17268 ) ;
#3280 = DIRECTION ( 'NONE',  ( 0.000000000000000000, -1.000000000000000000, 0.000000000000000000 ) ) ;
#3281 = EDGE_CURVE ( 'NONE', #10285, #27697, #26871, .T. ) ;
#3282 = VERTEX_POINT ( 'NONE', #16111 ) ;
#3283 = ORIENTED_EDGE ( 'NONE', *, *, #1605, .T. ) ;
#3284 = AXIS2_PLACEMENT_3D ( 'NONE', #3500, #3782, #21026 ) ;
#3285 =( GEOMETRIC_REPRESENTATION_CONTEXT ( 3 ) GLOBAL_UNCERTAINTY_ASSIGNED_CONTEXT ( ( #15803 ) ) GLOBAL_UNIT_ASSIGNED_CONTEXT ( ( #5516, #19150, #3633 ) ) REPRESENTATION_CONTEXT ( 'NONE', 'WORKASPACE' ) );
#3286 = ORIENTED_EDGE ( 'NONE', *, *, #11806, .T. ) ;
#3287 = TOROIDAL_SURFACE ( 'NONE', #25764, 18.46313063346208239, 2.000000000000000000 ) ;
#3288 = EDGE_LOOP ( 'NONE', ( #12041, #27248, #2971, #24568 ) ) ;
#3289 = ORIENTED_EDGE ( 'NONE', *, *, #9470, .F. ) ;
#3290 = LINE ( 'NONE', #9357, #13528 ) ;
#3291 = CARTESIAN_POINT ( 'NONE',  ( -175.0000000000000000, -120.0000000000001705, 70.00000000000001421 ) ) ;
#3292 = DIRECTION ( 'NONE',  ( -0.000000000000000000, -0.000000000000000000, -1.000000000000000000 ) ) ;
#3293 = CARTESIAN_POINT ( 'NONE',  ( 99.70648414290917572, 234.7927111797802695, -22.37570813572899553 ) ) ;
#3294 = CARTESIAN_POINT ( 'NONE',  ( 217.4999999999996305, 133.0668745871126930, -42.86484227207692044 ) ) ;
#3295 = AXIS2_PLACEMENT_3D ( 'NONE', #22146, #26589, #17410 ) ;
#3296 = CARTESIAN_POINT ( 'NONE',  ( -210.0000000000000568, -280.0000000000000000, -110.0000000000000284 ) ) ;
#3297 = VECTOR ( 'NONE', #14092, 1000.000000000000000 ) ;
#3298 = PLANE ( 'NONE',  #10930 ) ;
#3299 = CARTESIAN_POINT ( 'NONE',  ( -218.7748983233592526, 71.27581659157533522, -22.75434709466339100 ) ) ;
#3300 = EDGE_CURVE ( 'NONE', #7395, #1554, #9777, .T. ) ;
#3301 = AXIS2_PLACEMENT_3D ( 'NONE', #14465, #10717, #16760 ) ;
#3302 = ADVANCED_FACE ( 'NONE', ( #27283 ), #20403, .F. ) ;
#3303 = DIRECTION ( 'NONE',  ( 0.000000000000000000, 0.000000000000000000, -1.000000000000000000 ) ) ;
#3304 = DIRECTION ( 'NONE',  ( 1.000000000000000000, 4.625929269271485914E-16, 0.000000000000000000 ) ) ;
#3305 = LINE ( 'NONE', #12099, #4692 ) ;
#3306 = FACE_OUTER_BOUND ( 'NONE', #14305, .T. ) ;
#3307 = ORIENTED_EDGE ( 'NONE', *, *, #6883, .T. ) ;
#3308 = CARTESIAN_POINT ( 'NONE',  ( -254.4816742664885965, 103.7585653882801182, -5.000000000000004441 ) ) ;
#3309 = EDGE_CURVE ( 'NONE', #7097, #3365, #25132, .T. ) ;
#3310 = EDGE_CURVE ( 'NONE', #2723, #28076, #12080, .T. ) ;
#3311 = PLANE ( 'NONE',  #21814 ) ;
#3312 = ORIENTED_EDGE ( 'NONE', *, *, #18313, .F. ) ;
#3313 = ORIENTED_EDGE ( 'NONE', *, *, #1174, .F. ) ;
#3314 = VECTOR ( 'NONE', #26838, 1000.000000000000000 ) ;
#3315 = EDGE_LOOP ( 'NONE', ( #298, #4278, #7540, #20495 ) ) ;
#3316 = PRODUCT_DEFINITION ( 'UNKNOWN', '', #4206, #7165 ) ;
#3317 = VECTOR ( 'NONE', #19745, 1000.000000000000000 ) ;
#3318 = LINE ( 'NONE', #16414, #20270 ) ;
#3319 = CARTESIAN_POINT ( 'NONE',  ( 157.9999999999998579, 221.0000000000000284, 45.00000000000000000 ) ) ;
#3320 = ORIENTED_EDGE ( 'NONE', *, *, #11587, .T. ) ;
#3321 = VECTOR ( 'NONE', #1088, 1000.000000000000000 ) ;
#3322 = ORIENTED_EDGE ( 'NONE', *, *, #10106, .F. ) ;
#3323 = FACE_OUTER_BOUND ( 'NONE', #6619, .T. ) ;
#3324 = VECTOR ( 'NONE', #12427, 1000.000000000000000 ) ;
#3325 = CARTESIAN_POINT ( 'NONE',  ( -212.2419371577844345, -220.0000000000000853, -105.0000000000000284 ) ) ;
#3326 = DIRECTION ( 'NONE',  ( 1.387778780781444413E-14, 1.000000000000000000, 0.000000000000000000 ) ) ;
#3327 = VERTEX_POINT ( 'NONE', #22393 ) ;
#3328 = CARTESIAN_POINT ( 'NONE',  ( 209.9999999999999432, -150.0000000000000284, 110.0000000000000284 ) ) ;
#3329 = VERTEX_POINT ( 'NONE', #17790 ) ;
#3330 = FACE_OUTER_BOUND ( 'NONE', #22023, .T. ) ;
#3331 = DIRECTION ( 'NONE',  ( 0.000000000000000000, -1.000000000000000000, 0.000000000000000000 ) ) ;
#3332 = LINE ( 'NONE', #9678, #8007 ) ;
#3333 = EDGE_CURVE ( 'NONE', #17412, #14898, #11491, .T. ) ;
#3334 = CARTESIAN_POINT ( 'NONE',  ( -43.04748092857122543, 38.65804596583237895, 45.00000000000000000 ) ) ;
#3335 = FACE_OUTER_BOUND ( 'NONE', #6771, .T. ) ;
#3336 = VECTOR ( 'NONE', #18884, 1000.000000000000000 ) ;
#3337 = CARTESIAN_POINT ( 'NONE',  ( 157.9999999999999147, 215.9842499849850697, -45.00000000000000000 ) ) ;
#3338 = CARTESIAN_POINT ( 'NONE',  ( 163.4559080432011058, 210.4994054145057021, -145.3931298709317730 ) ) ;
#3339 = EDGE_CURVE ( 'NONE', #20334, #27997, #18371, .T. ) ;
#3340 = VERTEX_POINT ( 'NONE', #563 ) ;
#3341 = AXIS2_PLACEMENT_3D ( 'NONE', #22300, #21733, #24034 ) ;
#3342 = DIRECTION ( 'NONE',  ( -0.7440215159219069063, -0.6681556583950086781, 0.000000000000000000 ) ) ;
#3343 = LINE ( 'NONE', #10247, #5075 ) ;
#3344 = CARTESIAN_POINT ( 'NONE',  ( 157.4999999999996589, 276.4271876689075498, -45.00000000000000000 ) ) ;
#3345 = AXIS2_PLACEMENT_3D ( 'NONE', #5821, #12027, #12311 ) ;
#3346 = LINE ( 'NONE', #20460, #13963 ) ;
#3347 = ORIENTED_EDGE ( 'NONE', *, *, #12084, .F. ) ;
#3348 = LINE ( 'NONE', #22476, #11906 ) ;
#3349 = AXIS2_PLACEMENT_3D ( 'NONE', #25379, #1386, #5699 ) ;
#3350 = VERTEX_POINT ( 'NONE', #24402 ) ;
#3351 = EDGE_CURVE ( 'NONE', #12823, #2799, #13356, .T. ) ;
#3352 = DIRECTION ( 'NONE',  ( 0.000000000000000000, 0.000000000000000000, -1.000000000000000000 ) ) ;
#3353 = PLANE ( 'NONE',  #2296 ) ;
#3354 = CARTESIAN_POINT ( 'NONE',  ( 158.0000000000008811, 123.1928747072253572, 45.00000000000000000 ) ) ;
#3355 = ORIENTED_EDGE ( 'NONE', *, *, #3106, .T. ) ;
#3356 = DIRECTION ( 'NONE',  ( 0.000000000000000000, -1.000000000000000000, 0.000000000000000000 ) ) ;
#3357 = ORIENTED_EDGE ( 'NONE', *, *, #2688, .F. ) ;
#3358 = EDGE_CURVE ( 'NONE', #19001, #4212, #11344, .T. ) ;
#3359 = CARTESIAN_POINT ( 'NONE',  ( -138.1489073431982320, 127.5559642418054267, 17.69987763149199722 ) ) ;
#3360 = DIRECTION ( 'NONE',  ( 0.4528218681379916899, 0.8916010070295005141, -0.000000000000000000 ) ) ;
#3361 = EDGE_LOOP ( 'NONE', ( #9405, #14442, #28120, #24244 ) ) ;
#3362 = CONICAL_SURFACE ( 'NONE', #6586, 6.025000000000002132, 0.7853981633974482790 ) ;
#3363 = ORIENTED_EDGE ( 'NONE', *, *, #15631, .T. ) ;
#3364 = CARTESIAN_POINT ( 'NONE',  ( -24.33210486176665910, 0.000000000000000000, 99.00000000000000000 ) ) ;
#3365 = VERTEX_POINT ( 'NONE', #22247 ) ;
#3366 = AXIS2_PLACEMENT_3D ( 'NONE', #19576, #26175, #15703 ) ;
#3367 = VERTEX_POINT ( 'NONE', #13645 ) ;
#3368 = VERTEX_POINT ( 'NONE', #9476 ) ;
#3369 = VECTOR ( 'NONE', #15588, 1000.000000000000000 ) ;
#3370 = ADVANCED_FACE ( 'NONE', ( #9039 ), #26545, .T. ) ;
#3371 = DIRECTION ( 'NONE',  ( -0.000000000000000000, 0.000000000000000000, -1.000000000000000000 ) ) ;
#3372 = DIRECTION ( 'NONE',  ( 1.000000000000000000, -0.000000000000000000, -0.000000000000000000 ) ) ;
#3373 = CARTESIAN_POINT ( 'NONE',  ( 134.9999999999998579, 455.5353319318992362, -145.0000000000000000 ) ) ;
#3374 = CARTESIAN_POINT ( 'NONE',  ( 90.17595424773269031, 111.7661400908363731, -72.22656249986501109 ) ) ;
#3375 = DIRECTION ( 'NONE',  ( -0.000000000000000000, -1.000000000000000000, -0.000000000000000000 ) ) ;
#3376 = ADVANCED_FACE ( 'NONE', ( #22106 ), #6876, .F. ) ;
#3377 = DIRECTION ( 'NONE',  ( 0.000000000000000000, 0.000000000000000000, -1.000000000000000000 ) ) ;
#3378 = DIRECTION ( 'NONE',  ( -0.000000000000000000, -0.000000000000000000, 1.000000000000000000 ) ) ;
#3379 = CARTESIAN_POINT ( 'NONE',  ( 65.00000000000000000, -120.0000000000000711, 64.00000000000002842 ) ) ;
#3380 = CARTESIAN_POINT ( 'NONE',  ( -1.445038208015836378E-15, -1.249999999999998890, -7.096885197977455206 ) ) ;
#3381 = CARTESIAN_POINT ( 'NONE',  ( 158.0000000000005969, 148.7794997898028271, -45.00000000000000000 ) ) ;
#3382 = ORIENTED_EDGE ( 'NONE', *, *, #14777, .F. ) ;
#3383 = VECTOR ( 'NONE', #15301, 1000.000000000000000 ) ;
#3384 = CARTESIAN_POINT ( 'NONE',  ( -13.28039411106728629, 129.6310766613705709, 16.84488389623813376 ) ) ;
#3385 = DIRECTION ( 'NONE',  ( -0.000000000000000000, -0.000000000000000000, 1.000000000000000000 ) ) ;
#3386 = LINE ( 'NONE', #3668, #10307 ) ;
#3387 = PLANE ( 'NONE',  #7430 ) ;
#3388 = AXIS2_PLACEMENT_3D ( 'NONE', #9930, #8873, #4275 ) ;
#3389 = ORIENTED_EDGE ( 'NONE', *, *, #3390, .T. ) ;
#3390 = EDGE_CURVE ( 'NONE', #8705, #25194, #26980, .T. ) ;
#3391 = EDGE_CURVE ( 'NONE', #24175, #3560, #15656, .T. ) ;
#3392 = CARTESIAN_POINT ( 'NONE',  ( 157.4999999999998579, 75.79718706834503905, 45.00000000000000000 ) ) ;
#3393 = ORIENTED_EDGE ( 'NONE', *, *, #12066, .T. ) ;
#3394 = DIRECTION ( 'NONE',  ( 0.000000000000000000, 0.000000000000000000, -1.000000000000000000 ) ) ;
#3395 = ORIENTED_EDGE ( 'NONE', *, *, #12329, .F. ) ;
#3396 = ORIENTED_EDGE ( 'NONE', *, *, #5098, .F. ) ;
#3397 = EDGE_LOOP ( 'NONE', ( #27837, #13204, #25032, #12686 ) ) ;
#3398 = VERTEX_POINT ( 'NONE', #27124 ) ;
#3399 = CARTESIAN_POINT ( 'NONE',  ( 157.4999999999998295, 231.2854375337815327, 45.00000000000000000 ) ) ;
#3400 = VECTOR ( 'NONE', #7057, 1000.000000000000000 ) ;
#3401 = EDGE_CURVE ( 'NONE', #25274, #17486, #27497, .T. ) ;
#3402 = DIRECTION ( 'NONE',  ( 0.000000000000000000, -0.000000000000000000, -1.000000000000000000 ) ) ;
#3403 = DIRECTION ( 'NONE',  ( 0.000000000000000000, -0.000000000000000000, -1.000000000000000000 ) ) ;
#3404 = CARTESIAN_POINT ( 'NONE',  ( -96.57547103839915792, 136.1729178183695694, -13.53436789263006190 ) ) ;
#3405 = VECTOR ( 'NONE', #9865, 1000.000000000000000 ) ;
#3406 = EDGE_CURVE ( 'NONE', #26858, #28003, #5000, .T. ) ;
#3407 = EDGE_CURVE ( 'NONE', #3147, #8779, #22883, .T. ) ;
#3408 = CARTESIAN_POINT ( 'NONE',  ( -213.4823095283139196, 56.20074567116226660, 41.47858424781075115 ) ) ;
#3409 = DIRECTION ( 'NONE',  ( -0.000000000000000000, -0.000000000000000000, -1.000000000000000000 ) ) ;
#3410 = CARTESIAN_POINT ( 'NONE',  ( 119.4436508138957720, 236.9705627484767376, 45.00000000000000000 ) ) ;
#3411 = DIRECTION ( 'NONE',  ( -0.000000000000000000, -0.000000000000000000, -1.000000000000000000 ) ) ;
#3412 = CARTESIAN_POINT ( 'NONE',  ( -24.92338318254761020, 127.6681916698425567, -151.0000000000000284 ) ) ;
#3413 = EDGE_CURVE ( 'NONE', #9316, #9313, #24547, .T. ) ;
#3414 = LINE ( 'NONE', #3129, #3708 ) ;
#3415 = FACE_OUTER_BOUND ( 'NONE', #6007, .T. ) ;
#3416 = DIRECTION ( 'NONE',  ( 1.000000000000000000, -0.000000000000000000, -0.000000000000000000 ) ) ;
#3417 = ORIENTED_EDGE ( 'NONE', *, *, #3562, .T. ) ;
#3418 = CARTESIAN_POINT ( 'NONE',  ( -277.2150368962633706, -170.0000000000001137, -90.47363622314027509 ) ) ;
#3419 = CARTESIAN_POINT ( 'NONE',  ( 119.7545560452836639, 132.4900181920934870, -100.0000000000000142 ) ) ;
#3420 = CARTESIAN_POINT ( 'NONE',  ( 158.0000000000006821, 138.7479997597746433, -45.00000000000000000 ) ) ;
#3422 = EDGE_LOOP ( 'NONE', ( #8605, #10326, #19321, #18529 ) ) ;
#3421 = ORIENTED_EDGE ( 'NONE', *, *, #26111, .T. ) ;
#3423 = VECTOR ( 'NONE', #134, 1000.000000000000000 ) ;
#3424 = CARTESIAN_POINT ( 'NONE',  ( 157.9999999999996305, 283.6968751876750616, 45.00000000000000000 ) ) ;
#3425 = ORIENTED_EDGE ( 'NONE', *, *, #8352, .F. ) ;
#3426 = VERTEX_POINT ( 'NONE', #9181 ) ;
#3427 = ADVANCED_FACE ( 'NONE', ( #24692 ), #13792, .T. ) ;
#3428 = AXIS2_PLACEMENT_3D ( 'NONE', #27338, #9833, #11858 ) ;
#3429 = ORIENTED_EDGE ( 'NONE', *, *, #9744, .F. ) ;
#3430 = ORIENTED_EDGE ( 'NONE', *, *, #16149, .T. ) ;
#3431 = EDGE_LOOP ( 'NONE', ( #15629, #17894 ) ) ;
#3432 = ORIENTED_EDGE ( 'NONE', *, *, #18706, .F. ) ;
#3433 = CARTESIAN_POINT ( 'NONE',  ( -175.0000000000000000, -120.0000000000001847, -69.99999999999998579 ) ) ;
#3434 = CARTESIAN_POINT ( 'NONE',  ( 157.4999999999997158, 263.8878126313725829, 45.00000000000000000 ) ) ;
#3435 = VECTOR ( 'NONE', #23064, 1000.000000000000000 ) ;
#3436 = CONICAL_SURFACE ( 'NONE', #8040, 30.00000000000001421, 0.4537856055185259252 ) ;
#3437 = SPHERICAL_SURFACE ( 'NONE', #2450, 30.00000000000000000 ) ;
#3438 = EDGE_CURVE ( 'NONE', #1247, #28076, #26690, .T. ) ;
#3439 = EDGE_CURVE ( 'NONE', #1554, #13479, #2847, .T. ) ;
#3440 = FACE_OUTER_BOUND ( 'NONE', #12942, .T. ) ;
#3441 = CARTESIAN_POINT ( 'NONE',  ( 158.0000000000009948, 110.6534996696901345, -45.00000000000000000 ) ) ;
#3442 = AXIS2_PLACEMENT_3D ( 'NONE', #23186, #14022, #23043 ) ;
#3443 = PLANE ( 'NONE',  #2699 ) ;
#3444 = CARTESIAN_POINT ( 'NONE',  ( -208.0931995358751863, 75.17094939810765197, -39.84805955944327138 ) ) ;
#3445 = CARTESIAN_POINT ( 'NONE',  ( 109.8358256782556452, 203.6659868461599388, -150.7960377432351606 ) ) ;
#3446 = CARTESIAN_POINT ( 'NONE',  ( 157.4999999999998579, 201.1909374436971802, 45.00000000000000000 ) ) ;
#3447 = CARTESIAN_POINT ( 'NONE',  ( -215.4886702565632390, 139.8420026707765942, -13.00000000000000178 ) ) ;
#3448 = FACE_OUTER_BOUND ( 'NONE', #16029, .T. ) ;
#3449 = ORIENTED_EDGE ( 'NONE', *, *, #25330, .F. ) ;
#3450 = CARTESIAN_POINT ( 'NONE',  ( 157.9999999999997726, 241.5708750675630370, 45.00000000000000000 ) ) ;
#3451 = EDGE_CURVE ( 'NONE', #18918, #10091, #26206, .T. ) ;
#3452 = CARTESIAN_POINT ( 'NONE',  ( 134.9999999999998579, 268.4896896257338881, -84.99999999999997158 ) ) ;
#3453 = ORIENTED_EDGE ( 'NONE', *, *, #27622, .F. ) ;
#3454 = VECTOR ( 'NONE', #15155, 1000.000000000000114 ) ;
#3455 = EDGE_LOOP ( 'NONE', ( #5249, #2055, #691, #19902 ) ) ;
#3456 = AXIS2_PLACEMENT_3D ( 'NONE', #9996, #8404, #21608 ) ;
#3457 = CIRCLE ( 'NONE', #12242, 29.99999999999997158 ) ;
#3458 = ORIENTED_EDGE ( 'NONE', *, *, #20779, .F. ) ;
#3459 = CARTESIAN_POINT ( 'NONE',  ( 158.0000000000005400, 153.7952498048169048, -45.00000000000000000 ) ) ;
#3460 = EDGE_CURVE ( 'NONE', #16717, #18830, #27813, .T. ) ;
#3461 = CARTESIAN_POINT ( 'NONE',  ( -6.124983682450844166E-17, 0.000000000000000000, 0.000000000000000000 ) ) ;
#3462 = ORIENTED_EDGE ( 'NONE', *, *, #12175, .T. ) ;
#3463 = B_SPLINE_CURVE_WITH_KNOTS ( 'NONE', 3,
 ( #8746, #1252, #16493, #18779, #23238, #23371, #3539, #3683, #12470, #8143, #21213, #16633, #21356, #10586, #1535, #14760, #25524, #10443, #23097, #19198, #27945, #10302, #12194, #8290 ),
 .UNSPECIFIED., .F., .F.,
 ( 4, 2, 2, 2, 2, 2, 2, 2, 2, 2, 2, 4 ),
 ( 0.006955041467238803551, 0.01003080572916759117, 0.01156868786013197543, 0.01310656999109636144, 0.01618233425302515599, 0.01772021638398955240, 0.01925809851495395228, 0.02233386277688266877, 0.02387174490784706865, 0.02540962703881146506, 0.02848539130074026482, 0.03156115556266906458 ),
 .UNSPECIFIED. ) ;
#3464 = AXIS2_PLACEMENT_3D ( 'NONE', #19455, #19595, #28197 ) ;
#3465 = ORIENTED_EDGE ( 'NONE', *, *, #2047, .T. ) ;
#3466 = CARTESIAN_POINT ( 'NONE',  ( -138.6428522700808230, 71.54464929955099706, 82.80879831960034210 ) ) ;
#3467 = CARTESIAN_POINT ( 'NONE',  ( 97.56710499309299678, 233.1474776945298117, 20.66392395443024554 ) ) ;
#3468 = FACE_OUTER_BOUND ( 'NONE', #28210, .T. ) ;
#3469 = ORIENTED_EDGE ( 'NONE', *, *, #18144, .F. ) ;
#3470 = EDGE_CURVE ( 'NONE', #21880, #27997, #25394, .T. ) ;
#3471 = CARTESIAN_POINT ( 'NONE',  ( 158.0000000000006537, 145.7637497747887210, -45.00000000000000000 ) ) ;
#3472 = ORIENTED_EDGE ( 'NONE', *, *, #26710, .T. ) ;
#3473 = CARTESIAN_POINT ( 'NONE',  ( 367.4999999999996021, -5.589247009368158103, 75.00000000000004263 ) ) ;
#3474 = EDGE_CURVE ( 'NONE', #2828, #24530, #21956, .T. ) ;
#3475 = EDGE_CURVE ( 'NONE', #3728, #10441, #23379, .T. ) ;
#3476 = DIRECTION ( 'NONE',  ( -0.9209112846414913012, -0.3897722486529259789, 0.000000000000000000 ) ) ;
#3477 = AXIS2_PLACEMENT_3D ( 'NONE', #16366, #27392, #3265 ) ;
#3478 = DIRECTION ( 'NONE',  ( -0.000000000000000000, -0.000000000000000000, -1.000000000000000000 ) ) ;
#3479 = CARTESIAN_POINT ( 'NONE',  ( 158.0000000000000000, 206.4606249624626457, 45.00000000000000000 ) ) ;
#3480 = CARTESIAN_POINT ( 'NONE',  ( 134.9999999999998579, 220.0000000000000284, 100.0000000000000142 ) ) ;
#3481 = VECTOR ( 'NONE', #17462, 1000.000000000000000 ) ;
#3482 = PLANE ( 'NONE',  #1859 ) ;
#3483 = CARTESIAN_POINT ( 'NONE',  ( 163.3519221325304898, 210.1932722521781045, -143.0657854549350532 ) ) ;
#3484 = ORIENTED_EDGE ( 'NONE', *, *, #2365, .F. ) ;
#3485 = DIRECTION ( 'NONE',  ( -0.000000000000000000, -1.000000000000000000, -0.000000000000000000 ) ) ;
#3487 = DIRECTION ( 'NONE',  ( -0.000000000000000000, -0.000000000000000000, -1.000000000000000000 ) ) ;
#3486 = AXIS2_PLACEMENT_3D ( 'NONE', #11054, #133, #15516 ) ;
#3488 = CARTESIAN_POINT ( 'NONE',  ( 134.9999999999998579, 220.0000000000000284, 90.00000000000002842 ) ) ;
#3489 = CARTESIAN_POINT ( 'NONE',  ( 158.0000000000015348, 60.49599951954928656, -45.00000000000000000 ) ) ;
#3490 = VERTEX_POINT ( 'NONE', #20802 ) ;
#3491 = DIRECTION ( 'NONE',  ( -0.000000000000000000, -0.000000000000000000, 1.000000000000000000 ) ) ;
#3492 = ORIENTED_EDGE ( 'NONE', *, *, #24622, .F. ) ;
#3493 = LINE ( 'NONE', #14020, #23551 ) ;
#3494 = DIRECTION ( 'NONE',  ( -0.000000000000000000, -1.000000000000000000, -0.000000000000000000 ) ) ;
#3495 = DIRECTION ( 'NONE',  ( 0.000000000000000000, 0.000000000000000000, 1.000000000000000000 ) ) ;
#3496 = VERTEX_POINT ( 'NONE', #9889 ) ;
#3497 = DIRECTION ( 'NONE',  ( 0.8916010070294503320, 0.4528218681380901667, 0.000000000000000000 ) ) ;
#3498 = DIRECTION ( 'NONE',  ( 1.000000000000000000, 0.000000000000000000, -0.000000000000000000 ) ) ;
#3499 = EDGE_LOOP ( 'NONE', ( #19416, #24121, #13915, #13198 ) ) ;
#3500 = CARTESIAN_POINT ( 'NONE',  ( 217.4999999999996305, 44.41075299063186321, -100.0000000000000142 ) ) ;
#3501 = LINE ( 'NONE', #7822, #15418 ) ;
#3502 = ORIENTED_EDGE ( 'NONE', *, *, #27503, .T. ) ;
#3503 = AXIS2_PLACEMENT_3D ( 'NONE', #11553, #22741, #5205 ) ;
#3504 = ORIENTED_EDGE ( 'NONE', *, *, #8822, .F. ) ;
#3505 = CARTESIAN_POINT ( 'NONE',  ( -110.3221550338875687, 20.24192588826928585, 83.00000000000001421 ) ) ;
#3506 = ORIENTED_EDGE ( 'NONE', *, *, #16241, .F. ) ;
#3507 = EDGE_CURVE ( 'NONE', #24186, #13425, #22959, .T. ) ;
#3508 = EDGE_LOOP ( 'NONE', ( #24713, #9489, #4551, #13021, #17287, #19091 ) ) ;
#3509 = TOROIDAL_SURFACE ( 'NONE', #4412, 80.00000000000000000, 30.00000000000000000 ) ;
#3510 = ORIENTED_EDGE ( 'NONE', *, *, #25914, .F. ) ;
#3511 = FACE_OUTER_BOUND ( 'NONE', #22148, .T. ) ;
#3512 = ADVANCED_FACE ( 'NONE', ( #1260 ), #16502, .F. ) ;
#3513 = CARTESIAN_POINT ( 'NONE',  ( -210.0000000000000568, -216.9546086794800317, 109.5971846486504404 ) ) ;
#3514 = CARTESIAN_POINT ( 'NONE',  ( -210.0000000000000000, -150.0000000000001990, -100.0000000000000142 ) ) ;
#3515 = CARTESIAN_POINT ( 'NONE',  ( 33.10302365956999182, 203.2034914284457159, -15.00000000000000000 ) ) ;
#3516 = CARTESIAN_POINT ( 'NONE',  ( 22.58950924271104554, 154.2349915562422780, 12.99999999999999822 ) ) ;
#3517 = EDGE_CURVE ( 'NONE', #3705, #4742, #23103, .T. ) ;
#3518 = CARTESIAN_POINT ( 'NONE',  ( 158.0000000000009948, 110.6534996696901345, 45.00000000000000000 ) ) ;
#3519 = CARTESIAN_POINT ( 'NONE',  ( 157.9999999999998010, 233.5393750375350237, -45.00000000000000000 ) ) ;
#3520 = DIRECTION ( 'NONE',  ( 1.000000000000000000, 0.000000000000000000, 2.775557561562887407E-16 ) ) ;
#3521 = DIRECTION ( 'NONE',  ( 0.000000000000000000, 1.000000000000000000, -1.224646799147353207E-16 ) ) ;
#3522 = AXIS2_PLACEMENT_3D ( 'NONE', #24892, #24609, #27178 ) ;
#3523 = EDGE_LOOP ( 'NONE', ( #17931, #11794, #13410, #15572 ) ) ;
#3524 = DIRECTION ( 'NONE',  ( 0.9985600561963481336, -0.05364526231780537141, 0.000000000000000000 ) ) ;
#3525 = CARTESIAN_POINT ( 'NONE',  ( 108.6430499291109300, 252.6779224945142062, -32.26435679400692180 ) ) ;
#3526 = CARTESIAN_POINT ( 'NONE',  ( 13.66561450649970944, 89.77986226977256479, 98.36120057361384283 ) ) ;
#3527 = FACE_OUTER_BOUND ( 'NONE', #22907, .T. ) ;
#3528 = ORIENTED_EDGE ( 'NONE', *, *, #22375, .F. ) ;
#3529 = DIRECTION ( 'NONE',  ( 0.2383857661250380344, 0.9711705445023436356, 0.000000000000000000 ) ) ;
#3530 = ORIENTED_EDGE ( 'NONE', *, *, #23525, .T. ) ;
#3531 = PLANE ( 'NONE',  #11762 ) ;
#3532 = B_SPLINE_CURVE_WITH_KNOTS ( 'NONE', 3,
 ( #25769, #19167, #15156, #23482, #23909, #2061 ),
 .UNSPECIFIED., .F., .F.,
 ( 4, 2, 4 ),
 ( 0.001556600976750998223, 0.001854275657213667883, 0.002151950337676337543 ),
 .UNSPECIFIED. ) ;
#3533 = ORIENTED_EDGE ( 'NONE', *, *, #16413, .F. ) ;
#3534 = ORIENTED_EDGE ( 'NONE', *, *, #17358, .F. ) ;
#3535 = CARTESIAN_POINT ( 'NONE',  ( -62.54230505217808656, 134.9219987258869651, 15.37840988405203291 ) ) ;
#3536 = EDGE_CURVE ( 'NONE', #1808, #23293, #22417, .T. ) ;
#3537 = EDGE_LOOP ( 'NONE', ( #24567, #26756, #26146, #13562 ) ) ;
#3538 = ORIENTED_EDGE ( 'NONE', *, *, #23405, .T. ) ;
#3539 = CARTESIAN_POINT ( 'NONE',  ( 113.4521041897136229, 226.4953945451709387, 97.56026172913377081 ) ) ;
#3540 = AXIS2_PLACEMENT_3D ( 'NONE', #3291, #1423, #18671 ) ;
#3541 = CARTESIAN_POINT ( 'NONE',  ( 158.0000000000001705, 190.9054999099155054, -45.00000000000000000 ) ) ;
#3542 = CARTESIAN_POINT ( 'NONE',  ( -68.57415822541635464, 24.64876300893806160, 95.00000000000000000 ) ) ;
#3543 = VECTOR ( 'NONE', #20510, 1000.000000000000227 ) ;
#3544 = PLANE ( 'NONE',  #19254 ) ;
#3545 = CARTESIAN_POINT ( 'NONE',  ( -277.2150368962633706, -170.0000000000001137, -90.47363622314027509 ) ) ;
#3546 = DIRECTION ( 'NONE',  ( 1.000000000000000000, 1.321694076934710155E-16, 0.000000000000000000 ) ) ;
#3547 = CARTESIAN_POINT ( 'NONE',  ( -269.2495632547581863, -170.4544034111251278, 88.54864639839837537 ) ) ;
#3548 = EDGE_CURVE ( 'NONE', #14563, #14477, #8151, .T. ) ;
#3549 = EDGE_CURVE ( 'NONE', #18668, #22380, #28356, .T. ) ;
#3550 = CARTESIAN_POINT ( 'NONE',  ( 130.2364926426604086, 249.6196707243893229, -148.6534330424975678 ) ) ;
#3551 = CARTESIAN_POINT ( 'NONE',  ( 158.0000000000007674, 133.2243747372535267, 45.00000000000000000 ) ) ;
#3552 = FILL_AREA_STYLE_COLOUR ( '', #511 ) ;
#3553 = CARTESIAN_POINT ( 'NONE',  ( 9.999999999999957367, -20.00000000000004974, 80.00000000000001421 ) ) ;
#3554 = CARTESIAN_POINT ( 'NONE',  ( -26.23654403271235225, 26.23654403271337543, -45.00000000000000000 ) ) ;
#3555 = ORIENTED_EDGE ( 'NONE', *, *, #12480, .T. ) ;
#3556 = VECTOR ( 'NONE', #12408, 1000.000000000000000 ) ;
#3557 = CARTESIAN_POINT ( 'NONE',  ( -36.17830286759925684, -18.63254119118422025, 99.96486317258090537 ) ) ;
#3558 = CARTESIAN_POINT ( 'NONE',  ( 95.20156243613460845, 83.09913198707280912, -100.0000000000000284 ) ) ;
#3560 = VERTEX_POINT ( 'NONE', #10030 ) ;
#3559 = ORIENTED_EDGE ( 'NONE', *, *, #15075, .F. ) ;
#3561 = VECTOR ( 'NONE', #21819, 1000.000000000000000 ) ;
#3562 = EDGE_CURVE ( 'NONE', #8486, #12219, #18648, .T. ) ;
#3563 = ADVANCED_FACE ( 'NONE', ( #14073 ), #12199, .T. ) ;
#3564 = CARTESIAN_POINT ( 'NONE',  ( 157.4999999999998579, 100.8759371434154701, -45.00000000000000000 ) ) ;
#3565 = EDGE_LOOP ( 'NONE', ( #7999, #9561, #19090, #1648 ) ) ;
#3566 = ORIENTED_EDGE ( 'NONE', *, *, #6435, .F. ) ;
#3567 = ORIENTED_EDGE ( 'NONE', *, *, #2527, .F. ) ;
#3568 = ORIENTED_EDGE ( 'NONE', *, *, #10775, .T. ) ;
#3569 = EDGE_CURVE ( 'NONE', #17818, #10126, #14487, .T. ) ;
#3570 = ORIENTED_EDGE ( 'NONE', *, *, #1441, .T. ) ;
#3571 = ORIENTED_EDGE ( 'NONE', *, *, #1096, .T. ) ;
#3572 = CARTESIAN_POINT ( 'NONE',  ( -2.081668171172168513E-14, 90.00000000000001421, 98.28427124746191623 ) ) ;
#3573 = AXIS2_PLACEMENT_3D ( 'NONE', #1406, #16784, #25676 ) ;
#3574 = AXIS2_PLACEMENT_3D ( 'NONE', #29, #26440, #11238 ) ;
#3575 = DIRECTION ( 'NONE',  ( -0.8916010070297643031, 0.4528218681374719390, 0.000000000000000000 ) ) ;
#3576 = CARTESIAN_POINT ( 'NONE',  ( 158.0000000000014495, 68.01962454207041731, 45.00000000000000000 ) ) ;
#3577 = CARTESIAN_POINT ( 'NONE',  ( -260.0000000000001137, -220.0000000000000853, 60.00000000000002132 ) ) ;
#3578 = APPLICATION_CONTEXT ( 'automotive_design' ) ;
#3579 = DIRECTION ( 'NONE',  ( -0.000000000000000000, -0.000000000000000000, -1.000000000000000000 ) ) ;
#3580 = CARTESIAN_POINT ( 'NONE',  ( 157.4999999999996305, 288.9665627064425735, -45.00000000000000000 ) ) ;
#3581 = CARTESIAN_POINT ( 'NONE',  ( 158.0000000000013074, 81.06687458711267880, 45.00000000000000000 ) ) ;
#3583 = CARTESIAN_POINT ( 'NONE',  ( 109.8320145249364259, 203.6683199386712602, -139.1927212198768586 ) ) ;
#3582 = AXIS2_PLACEMENT_3D ( 'NONE', #27371, #1383, #23501 ) ;
#3584 = DIRECTION ( 'NONE',  ( 1.000000000000000000, 8.673617379884036705E-17, 0.000000000000000000 ) ) ;
#3585 = CARTESIAN_POINT ( 'NONE',  ( 150.8670668058245212, 232.1752285801742630, 45.00000000000000000 ) ) ;
#3586 = FACE_OUTER_BOUND ( 'NONE', #20709, .T. ) ;
#3587 = ORIENTED_EDGE ( 'NONE', *, *, #2690, .F. ) ;
#3588 = CARTESIAN_POINT ( 'NONE',  ( -43.04748092857122543, 38.65804596583237895, -45.00000000000000000 ) ) ;
#3589 = VECTOR ( 'NONE', #250, 1000.000000000000000 ) ;
#3590 = AXIS2_PLACEMENT_3D ( 'NONE', #15942, #20233, #420 ) ;
#3591 = CARTESIAN_POINT ( 'NONE',  ( -266.4480630393687193, -165.8483660650564389, -109.6897131948989568 ) ) ;
#3592 = ORIENTED_EDGE ( 'NONE', *, *, #11348, .F. ) ;
#3593 = APPLICATION_PROTOCOL_DEFINITION ( 'draft international standard', 'automotive_design', 1998, #5603 ) ;
#3594 = ORIENTED_EDGE ( 'NONE', *, *, #2546, .F. ) ;
#3596 = EDGE_CURVE ( 'NONE', #5621, #6964, #20940, .T. ) ;
#3595 = EDGE_LOOP ( 'NONE', ( #18286, #18778, #13663, #19227, #11134 ) ) ;
#3597 = CARTESIAN_POINT ( 'NONE',  ( 116.3389527601132869, 113.0483370489294543, 100.0000000000000142 ) ) ;
#3598 = DIRECTION ( 'NONE',  ( -1.000000000000000000, 0.000000000000000000, 0.000000000000000000 ) ) ;
#3599 = ORIENTED_EDGE ( 'NONE', *, *, #7895, .T. ) ;
#3600 = ADVANCED_FACE ( 'NONE', ( #9754 ), #23244, .T. ) ;
#3601 = ORIENTED_EDGE ( 'NONE', *, *, #25333, .T. ) ;
#3602 = CARTESIAN_POINT ( 'NONE',  ( -210.0000000000000568, -152.0000000000000284, -110.0000000000000284 ) ) ;
#3603 = LINE ( 'NONE', #12539, #6998 ) ;
#3604 = AXIS2_PLACEMENT_3D ( 'NONE', #4755, #7064, #13687 ) ;
#3605 = CARTESIAN_POINT ( 'NONE',  ( -180.0000000000000284, -70.00000000000004263, -70.00000000000001421 ) ) ;
#3606 = ORIENTED_EDGE ( 'NONE', *, *, #18957, .F. ) ;
#3607 = CARTESIAN_POINT ( 'NONE',  ( 106.3487426207432804, 91.82653269718771583, 100.0000000000000142 ) ) ;
#3608 = ORIENTED_EDGE ( 'NONE', *, *, #11326, .F. ) ;
#3609 = CARTESIAN_POINT ( 'NONE',  ( 157.9999999999999432, 213.4763749774776045, 45.00000000000000000 ) ) ;
#3610 = AXIS2_PLACEMENT_3D ( 'NONE', #3237, #12026, #4230 ) ;
#3611 = FACE_OUTER_BOUND ( 'NONE', #25231, .T. ) ;
#3612 = LINE ( 'NONE', #1741, #5255 ) ;
#3613 = CARTESIAN_POINT ( 'NONE',  ( 115.1711027725237955, 217.3894761555985156, -45.00000000000000000 ) ) ;
#3614 = DIRECTION ( 'NONE',  ( 1.000000000000000000, 0.000000000000000000, 0.000000000000000000 ) ) ;
#3615 = VECTOR ( 'NONE', #23912, 1000.000000000000000 ) ;
#3616 = VECTOR ( 'NONE', #13110, 1000.000000000000114 ) ;
#3617 = CARTESIAN_POINT ( 'NONE',  ( 158.0000000000012506, 88.08262460212675649, 45.00000000000000000 ) ) ;
#3618 = CARTESIAN_POINT ( 'NONE',  ( 162.9423453941602702, 209.0802367224323746, -148.9571385985324810 ) ) ;
#3619 = ORIENTED_EDGE ( 'NONE', *, *, #8053, .F. ) ;
#3620 = EDGE_CURVE ( 'NONE', #27544, #17314, #12339, .T. ) ;
#3621 = CARTESIAN_POINT ( 'NONE',  ( -225.7036482868739427, -91.18033988749901653, 18.91107291867258411 ) ) ;
#3622 = DIRECTION ( 'NONE',  ( 0.000000000000000000, 0.000000000000000000, -1.000000000000000000 ) ) ;
#3623 = FACE_OUTER_BOUND ( 'NONE', #22567, .T. ) ;
#3624 = LINE ( 'NONE', #10250, #23125 ) ;
#3625 = VERTEX_POINT ( 'NONE', #25109 ) ;
#3626 = DIRECTION ( 'NONE',  ( -1.000000000000000000, 0.000000000000000000, -0.000000000000000000 ) ) ;
#3627 = ORIENTED_EDGE ( 'NONE', *, *, #16737, .T. ) ;
#3628 = VECTOR ( 'NONE', #785, 1000.000000000000000 ) ;
#3629 = DIRECTION ( 'NONE',  ( -0.000000000000000000, 1.000000000000000000, -1.387778780781445429E-16 ) ) ;
#3630 = DIRECTION ( 'NONE',  ( 1.000000000000000000, 0.000000000000000000, 0.000000000000000000 ) ) ;
#3631 = DIRECTION ( 'NONE',  ( 0.000000000000000000, -1.000000000000000000, 0.000000000000000000 ) ) ;
#3632 = VERTEX_POINT ( 'NONE', #5426 ) ;
#3633 =( NAMED_UNIT ( * ) SI_UNIT ( $, .STERADIAN. ) SOLID_ANGLE_UNIT ( ) );
#3634 = VECTOR ( 'NONE', #4747, 1000.000000000000000 ) ;
#3635 = CARTESIAN_POINT ( 'NONE',  ( 349.0018770490533484, 96.44595867864246941, -145.0000000000000000 ) ) ;
#3636 = EDGE_CURVE ( 'NONE', #9167, #10678, #5893, .T. ) ;
#3637 = ORIENTED_EDGE ( 'NONE', *, *, #27273, .F. ) ;
#3638 = EDGE_CURVE ( 'NONE', #13707, #2371, #24057, .T. ) ;
#3639 = EDGE_CURVE ( 'NONE', #22969, #27280, #17578, .T. ) ;
#3640 = VECTOR ( 'NONE', #17767, 1000.000000000000114 ) ;
#3641 = CARTESIAN_POINT ( 'NONE',  ( -210.0000000000000568, -210.8114316696540982, 90.00000000000002842 ) ) ;
#3642 = EDGE_CURVE ( 'NONE', #9971, #7332, #4637, .T. ) ;
#3643 = CARTESIAN_POINT ( 'NONE',  ( 179.9999999999999147, 494.4107529906318632, -84.99999999999997158 ) ) ;
#3644 = VERTEX_POINT ( 'NONE', #8816 ) ;
#3645 = VERTEX_POINT ( 'NONE', #15727 ) ;
#3646 = AXIS2_PLACEMENT_3D ( 'NONE', #18958, #19524, #3575 ) ;
#3647 = FACE_OUTER_BOUND ( 'NONE', #28052, .T. ) ;
#3648 = ORIENTED_EDGE ( 'NONE', *, *, #21408, .F. ) ;
#3649 = VERTEX_POINT ( 'NONE', #13151 ) ;
#3650 = ORIENTED_EDGE ( 'NONE', *, *, #19190, .T. ) ;
#3651 = CARTESIAN_POINT ( 'NONE',  ( -189.8086322075389774, 92.49158130768422836, 12.99999999999999822 ) ) ;
#3652 = AXIS2_PLACEMENT_3D ( 'NONE', #22728, #11389, #22440 ) ;
#3653 = CARTESIAN_POINT ( 'NONE',  ( -63.57415822541634043, -23.01420295945612082, 100.0000000000000000 ) ) ;
#3654 = DIRECTION ( 'NONE',  ( 1.000000000000000000, 0.000000000000000000, 0.000000000000000000 ) ) ;
#3655 = DIRECTION ( 'NONE',  ( 0.000000000000000000, 1.214306433183764966E-16, -1.000000000000000000 ) ) ;
#3656 = AXIS2_PLACEMENT_3D ( 'NONE', #24205, #4373, #23925 ) ;
#3657 = CARTESIAN_POINT ( 'NONE',  ( 65.00000000000000000, -120.0000000000000995, -69.99999999999998579 ) ) ;
#3658 = CARTESIAN_POINT ( 'NONE',  ( -217.7467898461132449, 60.55642267084816410, -12.19614748119898806 ) ) ;
#3659 = FACE_OUTER_BOUND ( 'NONE', #19649, .T. ) ;
#3660 = LINE ( 'NONE', #1925, #5134 ) ;
#3661 = DIRECTION ( 'NONE',  ( -0.000000000000000000, -0.000000000000000000, -1.000000000000000000 ) ) ;
#3662 = FACE_OUTER_BOUND ( 'NONE', #207, .T. ) ;
#3663 = ORIENTED_EDGE ( 'NONE', *, *, #5671, .F. ) ;
#3664 = CARTESIAN_POINT ( 'NONE',  ( 2.399999999999999911, 0.000000000000000000, 0.000000000000000000 ) ) ;
#3665 = ADVANCED_FACE ( 'NONE', ( #24477 ), #26336, .F. ) ;
#3666 = EDGE_CURVE ( 'NONE', #15219, #4484, #202, .T. ) ;
#3667 = CARTESIAN_POINT ( 'NONE',  ( 157.4999999999998579, 108.3995621659365867, -45.00000000000000000 ) ) ;
#3668 = CARTESIAN_POINT ( 'NONE',  ( 157.4999999999998579, 135.9861872485140850, -45.00000000000000000 ) ) ;
#3669 = CARTESIAN_POINT ( 'NONE',  ( 217.4999999999996305, 258.6181251126050711, -6.024999999999988809 ) ) ;
#3670 = ORIENTED_EDGE ( 'NONE', *, *, #19154, .F. ) ;
#3671 = CIRCLE ( 'NONE', #5973, 9.999999999999982236 ) ;
#3672 = CARTESIAN_POINT ( 'NONE',  ( 187.4999999999996305, 83.06687458711267880, 36.86484227207694175 ) ) ;
#3673 = ORIENTED_EDGE ( 'NONE', *, *, #23039, .F. ) ;
#3674 = EDGE_CURVE ( 'NONE', #24234, #24769, #1748, .T. ) ;
#3675 = CARTESIAN_POINT ( 'NONE',  ( 157.4999999999998579, 68.27356204582390831, 45.00000000000000000 ) ) ;
#3676 = ORIENTED_EDGE ( 'NONE', *, *, #9940, .T. ) ;
#3677 = ORIENTED_EDGE ( 'NONE', *, *, #15337, .F. ) ;
#3678 = CARTESIAN_POINT ( 'NONE',  ( -77.62175523848470959, 136.2553702788594592, 13.51932229135349495 ) ) ;
#3679 = AXIS2_PLACEMENT_3D ( 'NONE', #7678, #3494, #18866 ) ;
#3680 = EDGE_CURVE ( 'NONE', #18978, #12426, #15550, .T. ) ;
#3681 = ORIENTED_EDGE ( 'NONE', *, *, #22426, .T. ) ;
#3682 = ORIENTED_EDGE ( 'NONE', *, *, #11254, .T. ) ;
#3683 = CARTESIAN_POINT ( 'NONE',  ( 113.0497540245548009, 225.0442599269872233, 97.19889357486866288 ) ) ;
#3684 = LINE ( 'NONE', #21074, #13291 ) ;
#3685 = CARTESIAN_POINT ( 'NONE',  ( -137.5548842902434501, 129.0090337181558482, -15.70719399148576301 ) ) ;
#3686 = CARTESIAN_POINT ( 'NONE',  ( -266.9759726783797191, -165.5689182401532946, -89.18477089400076352 ) ) ;
#3687 = DIRECTION ( 'NONE',  ( -0.000000000000000000, -0.000000000000000000, -1.000000000000000000 ) ) ;
#3688 = CARTESIAN_POINT ( 'NONE',  ( 29.35687238133360211, -42.92577930318808654, 99.85888104713946234 ) ) ;
#3689 = CARTESIAN_POINT ( 'NONE',  ( -229.0218807171185631, 91.25446205539969924, -13.22975565712915191 ) ) ;
#3690 = VECTOR ( 'NONE', #27640, 999.9999999999998863 ) ;
#3691 = CARTESIAN_POINT ( 'NONE',  ( 158.0000000000005400, 156.3031248123239436, -45.00000000000000000 ) ) ;
#3692 = DIRECTION ( 'NONE',  ( 0.8916010070293515222, -0.4528218681382848443, 0.000000000000000000 ) ) ;
#3693 = DIRECTION ( 'NONE',  ( -0.000000000000000000, 1.000000000000000000, -1.387778780781445429E-16 ) ) ;
#3694 = CARTESIAN_POINT ( 'NONE',  ( -37.82257053376181233, 71.03850157808263077, 99.00000000000000000 ) ) ;
#3695 = CARTESIAN_POINT ( 'NONE',  ( 157.4999999999998579, 193.6673124211760353, 45.00000000000000000 ) ) ;
#3696 = ORIENTED_EDGE ( 'NONE', *, *, #20832, .F. ) ;
#3697 = VECTOR ( 'NONE', #8789, 1000.000000000000114 ) ;
#3698 = EDGE_CURVE ( 'NONE', #9601, #543, #22033, .T. ) ;
#3699 = DIRECTION ( 'NONE',  ( 0.000000000000000000, 0.000000000000000000, -1.000000000000000000 ) ) ;
#3700 = CARTESIAN_POINT ( 'NONE',  ( 106.6482032540381510, 210.1929095456142704, -146.9353207969096786 ) ) ;
#3702 = VERTEX_POINT ( 'NONE', #14768 ) ;
#3701 = VERTEX_POINT ( 'NONE', #10982 ) ;
#3703 = CARTESIAN_POINT ( 'NONE',  ( 103.5789823554392655, 245.2557385300870862, -18.86932834261562064 ) ) ;
#3704 = ORIENTED_EDGE ( 'NONE', *, *, #21821, .T. ) ;
#3705 = VERTEX_POINT ( 'NONE', #6664 ) ;
#3706 = VERTEX_POINT ( 'NONE', #20016 ) ;
#3707 = ADVANCED_FACE ( 'NONE', ( #4784 ), #23520, .F. ) ;
#3708 = VECTOR ( 'NONE', #3268, 1000.000000000000000 ) ;
#3709 = EDGE_CURVE ( 'NONE', #11369, #20037, #10498, .T. ) ;
#3710 = ORIENTED_EDGE ( 'NONE', *, *, #8134, .T. ) ;
#3711 = VERTEX_POINT ( 'NONE', #19876 ) ;
#3712 = ORIENTED_EDGE ( 'NONE', *, *, #7995, .T. ) ;
#3713 = CARTESIAN_POINT ( 'NONE',  ( 134.9999999999998579, 220.0000000000000284, 45.00000000000000000 ) ) ;
#3714 = VECTOR ( 'NONE', #24271, 1000.000000000000000 ) ;
#3715 = CYLINDRICAL_SURFACE ( 'NONE', #1357, 5.000000000000004441 ) ;
#3716 = DIRECTION ( 'NONE',  ( -0.000000000000000000, -0.000000000000000000, -1.000000000000000000 ) ) ;
#3717 = EDGE_CURVE ( 'NONE', #6540, #10285, #26468, .T. ) ;
#3718 = PLANE ( 'NONE',  #15616 ) ;
#3719 = EDGE_CURVE ( 'NONE', #3632, #18947, #24326, .T. ) ;
#3720 = CARTESIAN_POINT ( 'NONE',  ( -277.5942566850414437, -165.0000000000001705, -106.8315826960697450 ) ) ;
#3721 = DIRECTION ( 'NONE',  ( 1.000000000000000000, 0.000000000000000000, -0.000000000000000000 ) ) ;
#3722 = CARTESIAN_POINT ( 'NONE',  ( -207.5108889574473494, 75.59417117316073131, -44.26576816510100798 ) ) ;
#3723 = AXIS2_PLACEMENT_3D ( 'NONE', #20491, #11610, #22797 ) ;
#3724 = CARTESIAN_POINT ( 'NONE',  ( 112.0174213346884926, 200.7165890697358464, -148.0040471605077812 ) ) ;
#3725 = DIRECTION ( 'NONE',  ( 0.4528218681381114274, 0.8916010070294396739, -0.000000000000000000 ) ) ;
#3726 = CARTESIAN_POINT ( 'NONE',  ( 294.9233831825459902, 127.6681916698402830, -137.0000000000000000 ) ) ;
#3727 = LINE ( 'NONE', #27430, #23966 ) ;
#3728 = VERTEX_POINT ( 'NONE', #22322 ) ;
#3729 = VECTOR ( 'NONE', #22338, 1000.000000000000000 ) ;
#3730 = CARTESIAN_POINT ( 'NONE',  ( -201.6781708543087461, 93.98296363999494929, 30.47827602183687290 ) ) ;
#3731 = CONICAL_SURFACE ( 'NONE', #23475, 14.64217782292691261, 0.08885387018394190484 ) ;
#3732 = DIRECTION ( 'NONE',  ( 1.000000000000000000, 0.000000000000000000, 0.000000000000000000 ) ) ;
#3733 = ORIENTED_EDGE ( 'NONE', *, *, #13882, .T. ) ;
#3734 = ITEM_DEFINED_TRANSFORMATION ( 'NONE', 'NONE', #16613,  #10637 ) ;
#3735 = ORIENTED_EDGE ( 'NONE', *, *, #12256, .F. ) ;
#3736 = ORIENTED_EDGE ( 'NONE', *, *, #26187, .F. ) ;
#3737 = EDGE_CURVE ( 'NONE', #18655, #20571, #2680, .T. ) ;
#3738 = EDGE_CURVE ( 'NONE', #18572, #23905, #9106, .T. ) ;
#3739 = CARTESIAN_POINT ( 'NONE',  ( 96.92716526681839184, 115.1868982021709229, 100.0000000000216573 ) ) ;
#3740 = LINE ( 'NONE', #12111, #20474 ) ;
#3741 = ORIENTED_EDGE ( 'NONE', *, *, #1380, .F. ) ;
#3742 = ORIENTED_EDGE ( 'NONE', *, *, #34, .T. ) ;
#3743 = CARTESIAN_POINT ( 'NONE',  ( 158.0000000000013074, 81.06687458711267880, -45.00000000000000000 ) ) ;
#3744 = AXIS2_PLACEMENT_3D ( 'NONE', #15881, #2780, #28028 ) ;
#3745 = DIRECTION ( 'NONE',  ( 0.8916010070298664436, 0.4528218681372709331, 0.000000000000000000 ) ) ;
#3746 = DIRECTION ( 'NONE',  ( -0.000000000000000000, -0.000000000000000000, 1.000000000000000000 ) ) ;
#3747 = VERTEX_POINT ( 'NONE', #26616 ) ;
#3748 = CARTESIAN_POINT ( 'NONE',  ( 109.6721745451680334, 96.60743919220468001, 100.0000000000000142 ) ) ;
#3749 = ORIENTED_EDGE ( 'NONE', *, *, #15508, .F. ) ;
#3750 = VECTOR ( 'NONE', #10399, 1000.000000000000000 ) ;
#3751 = AXIS2_PLACEMENT_3D ( 'NONE', #12388, #8057, #21124 ) ;
#3752 = CYLINDRICAL_SURFACE ( 'NONE', #22641, 49.99999999999998579 ) ;
#3753 = EDGE_CURVE ( 'NONE', #2370, #22168, #26540, .T. ) ;
#3754 = COLOUR_RGB ( '',0.7921568627450980005, 0.8196078431372548767, 0.9333333333333333481 ) ;
#3755 = CARTESIAN_POINT ( 'NONE',  ( -175.8417606860892874, 246.9430296707336652, 15.00000000000000000 ) ) ;
#3756 = FACE_OUTER_BOUND ( 'NONE', #11512, .T. ) ;
#3757 = DIRECTION ( 'NONE',  ( -0.000000000000000000, 0.000000000000000000, -1.000000000000000000 ) ) ;
#3758 = CARTESIAN_POINT ( 'NONE',  ( 187.4999999999996305, 288.9665627064425166, -45.00000000000000000 ) ) ;
#3759 = ADVANCED_FACE ( 'NONE', ( #10449 ), #19207, .F. ) ;
#3760 = ADVANCED_FACE ( 'NONE', ( #1050 ), #20725, .F. ) ;
#3761 = LINE ( 'NONE', #9957, #17474 ) ;
#3762 = CARTESIAN_POINT ( 'NONE',  ( -188.6733706988670463, 104.1136723946300577, -32.77950115724235047 ) ) ;
#3763 = ORIENTED_EDGE ( 'NONE', *, *, #4876, .F. ) ;
#3764 = DIRECTION ( 'NONE',  ( 0.000000000000000000, 0.000000000000000000, -1.000000000000000000 ) ) ;
#3765 = ADVANCED_FACE ( 'NONE', ( #774 ), #3057, .F. ) ;
#3766 = DIRECTION ( 'NONE',  ( 0.000000000000000000, -1.000000000000000000, 0.000000000000000000 ) ) ;
#3767 = DIRECTION ( 'NONE',  ( 1.000000000000000000, 0.000000000000000000, -0.000000000000000000 ) ) ;
#3768 = CARTESIAN_POINT ( 'NONE',  ( -210.0000000000000568, -150.0000000000000853, 99.99999999999991473 ) ) ;
#3769 = ORIENTED_EDGE ( 'NONE', *, *, #15701, .F. ) ;
#3770 = AXIS2_PLACEMENT_3D ( 'NONE', #12055, #1120, #23102 ) ;
#3771 = CARTESIAN_POINT ( 'NONE',  ( 158.0000000000016200, 50.97237449702815582, 45.00000000000000000 ) ) ;
#3772 = AXIS2_PLACEMENT_3D ( 'NONE', #26442, #11092, #6637 ) ;
#3773 = DIRECTION ( 'NONE',  ( 1.000000000000000000, 0.000000000000000000, 0.000000000000000000 ) ) ;
#3774 = CARTESIAN_POINT ( 'NONE',  ( -33.99100231024505803, 128.1996048026844903, -17.41651714595930045 ) ) ;
#3775 = CARTESIAN_POINT ( 'NONE',  ( -227.7254947214920264, 90.48960550153041993, 13.48035701177004597 ) ) ;
#3776 = ORIENTED_EDGE ( 'NONE', *, *, #22140, .F. ) ;
#3777 = DIRECTION ( 'NONE',  ( 0.000000000000000000, 0.000000000000000000, -1.000000000000000000 ) ) ;
#3778 = CYLINDRICAL_SURFACE ( 'NONE', #23068, 10.00000000000000888 ) ;
#3779 = AXIS2_PLACEMENT_3D ( 'NONE', #6616, #19551, #8773 ) ;
#3780 = ORIENTED_EDGE ( 'NONE', *, *, #13513, .F. ) ;
#3781 = AXIS2_PLACEMENT_3D ( 'NONE', #27138, #24992, #22976 ) ;
#3782 = DIRECTION ( 'NONE',  ( 0.000000000000000000, 1.214306433183764966E-16, -1.000000000000000000 ) ) ;
#3783 = FACE_OUTER_BOUND ( 'NONE', #18224, .T. ) ;
#3784 = ORIENTED_EDGE ( 'NONE', *, *, #386, .F. ) ;
#3785 = EDGE_CURVE ( 'NONE', #26726, #689, #25048, .T. ) ;
#3786 = ORIENTED_EDGE ( 'NONE', *, *, #2679, .F. ) ;
#3787 = DIRECTION ( 'NONE',  ( 0.000000000000000000, 0.000000000000000000, -1.000000000000000000 ) ) ;
#3788 = ORIENTED_EDGE ( 'NONE', *, *, #6781, .T. ) ;
#3789 = VERTEX_POINT ( 'NONE', #9821 ) ;
#3790 = EDGE_LOOP ( 'NONE', ( #18605, #869, #6825, #26339 ) ) ;
#3791 = VECTOR ( 'NONE', #9849, 1000.000000000000000 ) ;
#3792 = LINE ( 'NONE', #25908, #18492 ) ;
#3793 = VECTOR ( 'NONE', #15027, 1000.000000000000000 ) ;
#3794 = DIRECTION ( 'NONE',  ( 0.000000000000000000, 0.000000000000000000, -1.000000000000000000 ) ) ;
#3795 = DIRECTION ( 'NONE',  ( -1.000000000000000000, 0.000000000000000000, 0.000000000000000000 ) ) ;
#3796 = LINE ( 'NONE', #12586, #21105 ) ;
#3797 = CIRCLE ( 'NONE', #19858, 18.46313063346208239 ) ;
#3798 = ADVANCED_FACE ( 'NONE', ( #3335 ), #7240, .F. ) ;
#3799 = CIRCLE ( 'NONE', #22158, 7.499999999999992895 ) ;
#3800 = EDGE_CURVE ( 'NONE', #11671, #11276, #911, .T. ) ;
#3801 = DIRECTION ( 'NONE',  ( 1.000000000000000000, 0.000000000000000000, 0.000000000000000000 ) ) ;
#3802 = CARTESIAN_POINT ( 'NONE',  ( -203.1779787704217313, 93.05164332230201296, 28.77272332722132120 ) ) ;
#3803 = CARTESIAN_POINT ( 'NONE',  ( -234.1955688336022092, 78.70261838805063803, -15.19002172608862899 ) ) ;
#3804 = ORIENTED_EDGE ( 'NONE', *, *, #22869, .F. ) ;
#3805 = ADVANCED_FACE ( 'NONE', ( #11706 ), #20451, .F. ) ;
#3806 = CARTESIAN_POINT ( 'NONE',  ( 158.0000000000007105, 138.2401247522676044, -45.00000000000000000 ) ) ;
#3807 = FACE_OUTER_BOUND ( 'NONE', #2226, .T. ) ;
#3808 = CARTESIAN_POINT ( 'NONE',  ( 134.9999999999998579, 220.0000000000000284, -100.0000000000000142 ) ) ;
#3809 = CARTESIAN_POINT ( 'NONE',  ( 158.0000000000000568, 203.4448749474510407, 45.00000000000000000 ) ) ;
#3810 = ORIENTED_EDGE ( 'NONE', *, *, #9140, .F. ) ;
#3811 = CARTESIAN_POINT ( 'NONE',  ( 0.000000000000000000, 196.9999999999997442, 45.00000000000000000 ) ) ;
#3812 = CARTESIAN_POINT ( 'NONE',  ( 2.399999999999999911, -1.250000000000000444, 7.582700855991164168 ) ) ;
#3813 = DIRECTION ( 'NONE',  ( 1.000000000000000000, -0.000000000000000000, -0.000000000000000000 ) ) ;
#3814 = CARTESIAN_POINT ( 'NONE',  ( 157.9999999999997442, 253.6023750975910502, 45.00000000000000000 ) ) ;
#3815 = VERTEX_POINT ( 'NONE', #18013 ) ;
#3816 = CIRCLE ( 'NONE', #19869, 15.26911010665567225 ) ;
#3817 = VECTOR ( 'NONE', #13161, 1000.000000000000114 ) ;
#3818 = CARTESIAN_POINT ( 'NONE',  ( -233.7137317802251175, 78.16591391987653026, 15.26566376705435069 ) ) ;
#3819 = EDGE_LOOP ( 'NONE', ( #27355, #16449, #19880 ) ) ;
#3820 = CARTESIAN_POINT ( 'NONE',  ( 157.4999999999996305, 286.4586876989355915, 45.00000000000000000 ) ) ;
#3821 = ORIENTED_EDGE ( 'NONE', *, *, #24249, .T. ) ;
#3822 = AXIS2_PLACEMENT_3D ( 'NONE', #10599, #3844, #27959 ) ;
#3823 = ORIENTED_EDGE ( 'NONE', *, *, #5826, .F. ) ;
#3824 = CARTESIAN_POINT ( 'NONE',  ( 157.9999999999997442, 249.0945000900840398, 45.00000000000000000 ) ) ;
#3825 = VERTEX_POINT ( 'NONE', #16153 ) ;
#3826 = ORIENTED_EDGE ( 'NONE', *, *, #14419, .F. ) ;
#3827 = FACE_OUTER_BOUND ( 'NONE', #114, .T. ) ;
#3828 = LINE ( 'NONE', #10445, #1349 ) ;
#3829 = FACE_OUTER_BOUND ( 'NONE', #21521, .T. ) ;
#3830 = CARTESIAN_POINT ( 'NONE',  ( -151.0466515240400440, 123.3377277206981120, -20.04773851805323659 ) ) ;
#3831 = AXIS2_PLACEMENT_3D ( 'NONE', #4036, #23304, #14688 ) ;
#3832 = EDGE_CURVE ( 'NONE', #26471, #23612, #24621, .T. ) ;
#3833 = CARTESIAN_POINT ( 'NONE',  ( 65.00000000000000000, -150.0000000000000568, 76.00000000000001421 ) ) ;
#3834 = DIRECTION ( 'NONE',  ( 0.8916010070296124246, -0.4528218681377710886, 0.000000000000000000 ) ) ;
#3835 = CARTESIAN_POINT ( 'NONE',  ( 18.30893690202339741, -48.84579300681143366, 98.66826089724658289 ) ) ;
#3836 = CARTESIAN_POINT ( 'NONE',  ( -231.3914616533584763, 93.02691812379475778, -12.99999999981396215 ) ) ;
#3837 = AXIS2_PLACEMENT_3D ( 'NONE', #4626, #21883, #13414 ) ;
#3838 = EDGE_CURVE ( 'NONE', #23391, #14420, #11983, .T. ) ;
#3839 = CARTESIAN_POINT ( 'NONE',  ( 132.3447116496838305, 249.8827672015449082, -139.6159404653925833 ) ) ;
#3840 = DIRECTION ( 'NONE',  ( -0.000000000000000000, 1.000000000000000000, -1.387778780781445429E-16 ) ) ;
#3841 = VECTOR ( 'NONE', #15312, 1000.000000000000114 ) ;
#3842 = PLANE ( 'NONE',  #22092 ) ;
#3843 = PLANE ( 'NONE',  #16875 ) ;
#3844 = DIRECTION ( 'NONE',  ( -0.000000000000000000, -0.000000000000000000, 1.000000000000000000 ) ) ;
#3845 = ORIENTED_EDGE ( 'NONE', *, *, #13749, .F. ) ;
#3846 = DIRECTION ( 'NONE',  ( 0.7123733896039575741, 0.6147814225729705262, -0.3384788859638410141 ) ) ;
#3847 = DIRECTION ( 'NONE',  ( 0.4528218681383106015, -0.8916010070293384215, 0.000000000000000000 ) ) ;
#3848 = CARTESIAN_POINT ( 'NONE',  ( 157.4751130497510303, 215.0130877889310455, -45.00000000000000000 ) ) ;
#3850 = ORIENTED_EDGE ( 'NONE', *, *, #17554, .T. ) ;
#3849 = ORIENTED_EDGE ( 'NONE', *, *, #22423, .T. ) ;
#3851 = CARTESIAN_POINT ( 'NONE',  ( 105.7038310726791650, 247.5990904218954540, -23.20200675068357299 ) ) ;
#3852 = ORIENTED_EDGE ( 'NONE', *, *, #19794, .F. ) ;
#3853 = EDGE_LOOP ( 'NONE', ( #11519, #4209, #23044, #8212 ) ) ;
#3854 = AXIS2_PLACEMENT_3D ( 'NONE', #4782, #346, #15872 ) ;
#3855 = ORIENTED_EDGE ( 'NONE', *, *, #2842, .T. ) ;
#3856 = ORIENTED_EDGE ( 'NONE', *, *, #11443, .F. ) ;
#3857 = AXIS2_PLACEMENT_3D ( 'NONE', #26170, #22295, #15848 ) ;
#3858 = VERTEX_POINT ( 'NONE', #27051 ) ;
#3859 = ORIENTED_EDGE ( 'NONE', *, *, #7580, .T. ) ;
#3860 = FACE_OUTER_BOUND ( 'NONE', #6967, .T. ) ;
#3861 = EDGE_CURVE ( 'NONE', #620, #4812, #5073, .T. ) ;
#3862 = LINE ( 'NONE', #28128, #27047 ) ;
#3863 = CARTESIAN_POINT ( 'NONE',  ( 158.0000000000008527, 123.7007497147323960, 45.00000000000000000 ) ) ;
#3864 = DIRECTION ( 'NONE',  ( 1.000000000000000000, 0.000000000000000000, 0.000000000000000000 ) ) ;
#3865 = EDGE_CURVE ( 'NONE', #23487, #2018, #24718, .T. ) ;
#3866 = VECTOR ( 'NONE', #13181, 1000.000000000000000 ) ;
#3867 = CARTESIAN_POINT ( 'NONE',  ( 157.4999999999998579, 50.71843699327460797, 45.00000000000000000 ) ) ;
#3868 = CARTESIAN_POINT ( 'NONE',  ( 157.4999999999998579, 93.35231212089433939, 45.00000000000000000 ) ) ;
#3869 = CARTESIAN_POINT ( 'NONE',  ( -208.6543519075750908, 74.78670680337248200, -37.88580841379594233 ) ) ;
#3870 = VECTOR ( 'NONE', #7383, 1000.000000000000227 ) ;
#3871 = ADVANCED_FACE ( 'NONE', ( #7093 ), #18440, .F. ) ;
#3872 = CARTESIAN_POINT ( 'NONE',  ( -26.99706921587402775, 129.1643607319973626, 16.99462959852061772 ) ) ;
#3873 = LINE ( 'NONE', #12662, #17378 ) ;
#3874 = CARTESIAN_POINT ( 'NONE',  ( 0.000000000000000000, -280.0000000000000000, 110.0000000000000284 ) ) ;
#3875 = DIRECTION ( 'NONE',  ( 0.000000000000000000, 0.000000000000000000, 1.000000000000000000 ) ) ;
#3876 = VECTOR ( 'NONE', #10463, 1000.000000000000000 ) ;
#3877 = ORIENTED_EDGE ( 'NONE', *, *, #27328, .T. ) ;
#3878 = CARTESIAN_POINT ( 'NONE',  ( 119.9999999999999147, 236.7705098312484893, -100.0000000000000284 ) ) ;
#3879 = LINE ( 'NONE', #13095, #7611 ) ;
#3880 = VERTEX_POINT ( 'NONE', #13717 ) ;
#3881 = ITEM_DEFINED_TRANSFORMATION ( 'NONE', 'NONE', #94,  #10637 ) ;
#3882 = VERTEX_POINT ( 'NONE', #7531 ) ;
#3883 = EDGE_CURVE ( 'NONE', #9161, #18691, #3146, .T. ) ;
#3884 = ORIENTED_EDGE ( 'NONE', *, *, #1882, .F. ) ;
#3885 = CARTESIAN_POINT ( 'NONE',  ( 113.0425250404539241, 213.0812361363525440, -45.00000000000000000 ) ) ;
#3886 = DIRECTION ( 'NONE',  ( 0.000000000000000000, 0.000000000000000000, 1.000000000000000000 ) ) ;
#3887 = VERTEX_POINT ( 'NONE', #14138 ) ;
#3888 = CIRCLE ( 'NONE', #18140, 5.000000000000000000 ) ;
#3889 = AXIS2_PLACEMENT_3D ( 'NONE', #2416, #21964, #19808 ) ;
#3890 = ORIENTED_EDGE ( 'NONE', *, *, #24573, .F. ) ;
#3891 = CARTESIAN_POINT ( 'NONE',  ( 79.99999999999991473, 80.00000000000001421, -100.0000000000000142 ) ) ;
#3892 = EDGE_CURVE ( 'NONE', #11526, #24469, #22887, .T. ) ;
#3893 = LINE ( 'NONE', #18842, #12982 ) ;
#3894 = FACE_OUTER_BOUND ( 'NONE', #522, .T. ) ;
#3895 = EDGE_LOOP ( 'NONE', ( #27175, #6055, #359, #11257 ) ) ;
#3896 = CARTESIAN_POINT ( 'NONE',  ( 111.0641325991587252, 99.15168937823351314, 100.0000000000000142 ) ) ;
#3897 = ORIENTED_EDGE ( 'NONE', *, *, #25902, .F. ) ;
#3898 = AXIS2_PLACEMENT_3D ( 'NONE', #73, #1658, #10715 ) ;
#3899 = CARTESIAN_POINT ( 'NONE',  ( 12.78000883847031588, 237.8887863075477469, 45.00000000000000000 ) ) ;
#3900 = CARTESIAN_POINT ( 'NONE',  ( 158.0000000000011937, 91.09837461714084839, -45.00000000000000000 ) ) ;
#3901 = DIRECTION ( 'NONE',  ( 0.8916010070295112833, 0.4528218681379702626, 0.000000000000000000 ) ) ;
#3902 = PLANE ( 'NONE',  #6914 ) ;
#3903 = VERTEX_POINT ( 'NONE', #7665 ) ;
#3904 = EDGE_CURVE ( 'NONE', #7140, #18691, #16429, .T. ) ;
#3905 = EDGE_CURVE ( 'NONE', #9382, #12221, #9402, .T. ) ;
#3906 = CYLINDRICAL_SURFACE ( 'NONE', #24238, 6.000000000000005329 ) ;
#3907 = LINE ( 'NONE', #28307, #4613 ) ;
#3908 = DIRECTION ( 'NONE',  ( 0.4528218681335642870, 0.8916010070317489378, -0.000000000000000000 ) ) ;
#3909 = FACE_OUTER_BOUND ( 'NONE', #1077, .T. ) ;
#3910 = VECTOR ( 'NONE', #14590, 999.9999999999998863 ) ;
#3911 = VERTEX_POINT ( 'NONE', #2774 ) ;
#3912 = AXIS2_PLACEMENT_3D ( 'NONE', #18204, #7282, #11887 ) ;
#3913 = CARTESIAN_POINT ( 'NONE',  ( 157.4999999999998579, 63.25781203080982351, -45.00000000000000000 ) ) ;
#3914 = LINE ( 'NONE', #15133, #13940 ) ;
#3915 = DIRECTION ( 'NONE',  ( -0.000000000000000000, -0.000000000000000000, -1.000000000000000000 ) ) ;
#3916 = CARTESIAN_POINT ( 'NONE',  ( -225.0835117808284451, 89.24749510747318482, 14.20199329800427002 ) ) ;
#3917 = ORIENTED_EDGE ( 'NONE', *, *, #27423, .F. ) ;
#3918 = CARTESIAN_POINT ( 'NONE',  ( -2.081668171172168513E-14, 79.99999999999998579, -70.00000000000001421 ) ) ;
#3919 = CIRCLE ( 'NONE', #11278, 2.586968381275096984 ) ;
#3920 = VERTEX_POINT ( 'NONE', #25459 ) ;
#3921 = EDGE_CURVE ( 'NONE', #1653, #4329, #14840, .T. ) ;
#3922 = ADVANCED_FACE ( 'NONE', ( #12548 ), #7801, .F. ) ;
#3923 = PLANE ( 'NONE',  #3284 ) ;
#3924 = CARTESIAN_POINT ( 'NONE',  ( -167.4464202405217463, 116.4377010620362967, -25.83866841605921749 ) ) ;
#3925 = ORIENTED_EDGE ( 'NONE', *, *, #13099, .F. ) ;
#3926 = EDGE_LOOP ( 'NONE', ( #4495, #12001, #18599, #329 ) ) ;
#3927 = ADVANCED_FACE ( 'NONE', ( #1189 ), #27743, .F. ) ;
#3928 = DIRECTION ( 'NONE',  ( -0.8660254037844326014, 0.5000000000000106581, 0.000000000000000000 ) ) ;
#3929 = ORIENTED_EDGE ( 'NONE', *, *, #9136, .F. ) ;
#3930 = CIRCLE ( 'NONE', #8536, 16.46313063346208239 ) ;
#3931 = ADVANCED_FACE ( 'NONE', ( #21289 ), #14556, .T. ) ;
#3932 = ORIENTED_EDGE ( 'NONE', *, *, #5069, .T. ) ;
#3933 = EDGE_LOOP ( 'NONE', ( #14131, #3253, #17856, #19936 ) ) ;
#3934 = CIRCLE ( 'NONE', #19994, 10.71881775658151170 ) ;
#3935 = LINE ( 'NONE', #7975, #16766 ) ;
#3936 = CARTESIAN_POINT ( 'NONE',  ( 4.491205691019747093, 138.9213844498120238, 13.09540051078805156 ) ) ;
#3937 = CYLINDRICAL_SURFACE ( 'NONE', #11944, 70.83858790703926900 ) ;
#3938 = AXIS2_PLACEMENT_3D ( 'NONE', #18516, #5292, #13795 ) ;
#3939 = DIRECTION ( 'NONE',  ( 0.000000000000000000, 0.000000000000000000, 1.000000000000000000 ) ) ;
#3940 = FACE_OUTER_BOUND ( 'NONE', #665, .T. ) ;
#3941 = CARTESIAN_POINT ( 'NONE',  ( -229.6735579984113258, 64.27833679895920227, -7.258985754582258920 ) ) ;
#3942 = ORIENTED_EDGE ( 'NONE', *, *, #20538, .T. ) ;
#3943 = DIRECTION ( 'NONE',  ( 1.000000000000000000, 0.000000000000000000, -0.000000000000000000 ) ) ;
#3944 = CARTESIAN_POINT ( 'NONE',  ( 157.9999999999998579, 221.5078750075070104, 45.00000000000000000 ) ) ;
#3945 = CARTESIAN_POINT ( 'NONE',  ( -180.0000000000000284, -40.00000000000004974, -70.00000000000001421 ) ) ;
#3946 = CARTESIAN_POINT ( 'NONE',  ( 158.0000000000011937, 91.09837461714084839, 45.00000000000000000 ) ) ;
#3947 = ORIENTED_EDGE ( 'NONE', *, *, #18957, .T. ) ;
#3948 = LINE ( 'NONE', #6110, #6810 ) ;
#3949 = FACE_OUTER_BOUND ( 'NONE', #13104, .T. ) ;
#3950 = CARTESIAN_POINT ( 'NONE',  ( -260.0000000000001137, -167.0819201924624906, 90.00000000000001421 ) ) ;
#3951 = FACE_OUTER_BOUND ( 'NONE', #15568, .T. ) ;
#3952 = SURFACE_SIDE_STYLE ('',( #17737 ) ) ;
#3953 = CARTESIAN_POINT ( 'NONE',  ( 58.09044720719344213, 216.7965004116395562, -45.00000000000000000 ) ) ;
#3954 = ORIENTED_EDGE ( 'NONE', *, *, #22390, .F. ) ;
#3955 = CIRCLE ( 'NONE', #1214, 14.64217782292691261 ) ;
#3956 = CARTESIAN_POINT ( 'NONE',  ( -50.01279441628821587, 86.62470095750859400, 45.00000000000000000 ) ) ;
#3957 = ORIENTED_EDGE ( 'NONE', *, *, #3032, .T. ) ;
#3958 = CARTESIAN_POINT ( 'NONE',  ( 157.4999999999996874, 266.3956876388795649, -45.00000000000000000 ) ) ;
#3959 = ORIENTED_EDGE ( 'NONE', *, *, #6027, .F. ) ;
#3960 = VECTOR ( 'NONE', #8586, 1000.000000000000000 ) ;
#3961 = EDGE_CURVE ( 'NONE', #8160, #3252, #16412, .T. ) ;
#3962 = ORIENTED_EDGE ( 'NONE', *, *, #22705, .F. ) ;
#3963 = EDGE_CURVE ( 'NONE', #366, #2661, #1269, .T. ) ;
#3964 = CARTESIAN_POINT ( 'NONE',  ( -67.54154682840413670, 135.5235962012238815, 15.28890748345223116 ) ) ;
#3965 = ORIENTED_EDGE ( 'NONE', *, *, #5540, .F. ) ;
#3966 = EDGE_LOOP ( 'NONE', ( #11123, #5162, #4735, #15504 ) ) ;
#3967 = FACE_OUTER_BOUND ( 'NONE', #3029, .T. ) ;
#3968 = CARTESIAN_POINT ( 'NONE',  ( -160.0000000000000284, 119.7660240611718905, -22.85081902853004721 ) ) ;
#3969 = DIRECTION ( 'NONE',  ( 1.321694076934710155E-16, -1.000000000000000000, 0.000000000000000000 ) ) ;
#3970 = CARTESIAN_POINT ( 'NONE',  ( -127.6926693028035089, 131.7039880331085158, -16.10276958539054704 ) ) ;
#3971 = VECTOR ( 'NONE', #11595, 1000.000000000000000 ) ;
#3972 = CARTESIAN_POINT ( 'NONE',  ( -268.8456629416622263, -165.3150191422601551, -88.69519881272435669 ) ) ;
#3973 = CARTESIAN_POINT ( 'NONE',  ( -263.9427288773140390, -171.3087732700370225, 94.90640018636418063 ) ) ;
#3974 = CARTESIAN_POINT ( 'NONE',  ( -221.8631419436352985, 88.28315383663137084, -15.48010842192074854 ) ) ;
#3975 = CARTESIAN_POINT ( 'NONE',  ( 130.2301963871595945, 249.6192082491895974, -141.3391815462162810 ) ) ;
#3976 = CARTESIAN_POINT ( 'NONE',  ( -228.3351344443410653, 88.50822704663181639, 15.59479036512446370 ) ) ;
#3977 = FACE_OUTER_BOUND ( 'NONE', #18018, .T. ) ;
#3978 = DIRECTION ( 'NONE',  ( 0.000000000000000000, 0.000000000000000000, 1.000000000000000000 ) ) ;
#3979 = DIRECTION ( 'NONE',  ( 0.000000000000000000, -0.000000000000000000, -1.000000000000000000 ) ) ;
#3980 = ORIENTED_EDGE ( 'NONE', *, *, #18992, .T. ) ;
#3981 = EDGE_CURVE ( 'NONE', #10749, #23784, #18763, .T. ) ;
#3982 = PLANE ( 'NONE',  #26133 ) ;
#3983 = DIRECTION ( 'NONE',  ( -0.8916010070293383105, -0.4528218681383106015, 0.000000000000000000 ) ) ;
#3984 = B_SPLINE_CURVE_WITH_KNOTS ( 'NONE', 3,
 ( #12540, #6478, #10654, #21713, #2024, #10799, #19556, #8641, #1457, #5909, #14684, #21280, #10370, #27868, #8211, #14833, #16976, #6052, #23584, #21421, #1735, #10511, #2734, #19978, #2590, #17535 ),
 .UNSPECIFIED., .F., .F.,
 ( 4, 2, 2, 2, 2, 2, 2, 2, 2, 2, 2, 2, 4 ),
 ( 0.000000000000000000, 0.006543047306792185158, 0.01308609461358437032, 0.01962914192037655201, 0.02617218922716874063, 0.02944371288056481933, 0.03107947470726283787, 0.03271523653396085640, 0.03598676018735695592, 0.03925828384075306238, 0.04580133114754529611, 0.04907285480094141644, 0.05234437845433753678 ),
 .UNSPECIFIED. ) ;
#3985 = CARTESIAN_POINT ( 'NONE',  ( -112.3221550338875687, 22.24192588826928585, 83.00000000000001421 ) ) ;
#3987 = EDGE_LOOP ( 'NONE', ( #39, #13071, #2395, #4610 ) ) ;
#3986 = VERTEX_POINT ( 'NONE', #27878 ) ;
#3988 = CARTESIAN_POINT ( 'NONE',  ( 99.07849735471324948, 234.2556710009628489, -21.83147064533557113 ) ) ;
#3989 = EDGE_LOOP ( 'NONE', ( #578, #18448, #17971 ) ) ;
#3990 = ORIENTED_EDGE ( 'NONE', *, *, #6896, .T. ) ;
#3991 = EDGE_CURVE ( 'NONE', #10126, #21270, #12690, .T. ) ;
#3992 = AXIS2_PLACEMENT_3D ( 'NONE', #6903, #871, #15832 ) ;
#3993 = ORIENTED_EDGE ( 'NONE', *, *, #11307, .F. ) ;
#3994 = EDGE_CURVE ( 'NONE', #5384, #18983, #8612, .T. ) ;
#3996 = CLOSED_SHELL ( 'NONE', ( #238, #10166, #22536, #16043, #17421, #2843, #6982, #24610, #18673, #17163, #2172, #4904, #27874, #18220, #23426, #4744, #19820, #15702, #472, #22099, #11379, #22428, #2750, #12885, #26047, #15496 ) ) ;
#3995 = ADVANCED_FACE ( 'NONE', ( #12268 ), #1742, .T. ) ;
#3997 = EDGE_CURVE ( 'NONE', #2768, #11694, #14692, .T. ) ;
#3998 = ORIENTED_EDGE ( 'NONE', *, *, #28211, .T. ) ;
#3999 = EDGE_LOOP ( 'NONE', ( #6471, #2426, #10047, #5403 ) ) ;
#4000 = EDGE_LOOP ( 'NONE', ( #13487, #12109, #8141 ) ) ;
#4001 = LINE ( 'NONE', #12785, #9068 ) ;
#4002 = CARTESIAN_POINT ( 'NONE',  ( 158.0000000000007105, 138.2401247522676044, 45.00000000000000000 ) ) ;
#4003 = DIRECTION ( 'NONE',  ( -0.000000000000000000, 0.000000000000000000, -1.000000000000000000 ) ) ;
#4004 = CARTESIAN_POINT ( 'NONE',  ( 232.4999999999996305, 83.06687458711267880, 42.86484227207692754 ) ) ;
#4005 = CARTESIAN_POINT ( 'NONE',  ( -305.0000000000001137, -165.0000000000000853, -59.99999999999987210 ) ) ;
#4006 = DIRECTION ( 'NONE',  ( 1.000000000000000000, 0.000000000000000000, -0.000000000000000000 ) ) ;
#4007 = VECTOR ( 'NONE', #22680, 1000.000000000000000 ) ;
#4008 = CARTESIAN_POINT ( 'NONE',  ( -234.3956316663174277, 78.94038675297558427, -15.16326400926280904 ) ) ;
#4009 = CARTESIAN_POINT ( 'NONE',  ( -31.62490448008894361, 128.0247143377008285, 17.49372955826459020 ) ) ;
#4010 = CARTESIAN_POINT ( 'NONE',  ( 139.9869122110687840, 242.4751130497508314, 45.00000000000000000 ) ) ;
#4011 = LINE ( 'NONE', #3874, #16129 ) ;
#4012 = FACE_OUTER_BOUND ( 'NONE', #25102, .T. ) ;
#4013 = ORIENTED_EDGE ( 'NONE', *, *, #9061, .F. ) ;
#4014 = CARTESIAN_POINT ( 'NONE',  ( 134.9999999999998579, -327.2004514666934369, 84.99999999999995737 ) ) ;
#4015 = ADVANCED_FACE ( 'NONE', ( #18853 ), #1608, .F. ) ;
#4016 = ADVANCED_FACE ( 'NONE', ( #10377 ), #25591, .F. ) ;
#4017 = CARTESIAN_POINT ( 'NONE',  ( -271.2500882473517549, -165.3342412936102050, -108.7452232840771558 ) ) ;
#4018 = ORIENTED_EDGE ( 'NONE', *, *, #18662, .T. ) ;
#4019 = CONTEXT_DEPENDENT_SHAPE_REPRESENTATION ( #5053, #13049 ) ;
#4020 = ORIENTED_EDGE ( 'NONE', *, *, #16246, .T. ) ;
#4021 = ORIENTED_EDGE ( 'NONE', *, *, #21820, .T. ) ;
#4022 = VECTOR ( 'NONE', #23990, 1000.000000000000000 ) ;
#4023 = CARTESIAN_POINT ( 'NONE',  ( 117.1152841538673073, 116.0550883417529207, 100.0000000000000142 ) ) ;
#4024 = DIRECTION ( 'NONE',  ( 0.8916010070293283185, 0.4528218681383305855, 0.000000000000000000 ) ) ;
#4025 = ADVANCED_FACE ( 'NONE', ( #8221 ), #6060, .T. ) ;
#4026 = AXIS2_PLACEMENT_3D ( 'NONE', #8368, #19568, #8512 ) ;
#4027 = ORIENTED_EDGE ( 'NONE', *, *, #3800, .T. ) ;
#4028 = ORIENTED_EDGE ( 'NONE', *, *, #12389, .T. ) ;
#4029 = CARTESIAN_POINT ( 'NONE',  ( 85.90765579568754617, 110.5723347145559785, -100.0000000000000284 ) ) ;
#4030 = EDGE_CURVE ( 'NONE', #9386, #18364, #25734, .T. ) ;
#4031 = CARTESIAN_POINT ( 'NONE',  ( 96.79688798037243203, 232.6553591674251606, 20.12433470795689772 ) ) ;
#4032 = CARTESIAN_POINT ( 'NONE',  ( 158.0000000000007105, 138.2401247522676044, 45.00000000000000000 ) ) ;
#4033 = ORIENTED_EDGE ( 'NONE', *, *, #2219, .F. ) ;
#4034 = CARTESIAN_POINT ( 'NONE',  ( -228.1057710792337616, 90.70189914778829632, 15.47288924712567848 ) ) ;
#4035 = EDGE_LOOP ( 'NONE', ( #12323, #19079, #7438, #21841 ) ) ;
#4036 = CARTESIAN_POINT ( 'NONE',  ( 232.4999999999996305, 133.0668745871126930, 36.86484227207694886 ) ) ;
#4037 =( GEOMETRIC_REPRESENTATION_CONTEXT ( 3 ) GLOBAL_UNCERTAINTY_ASSIGNED_CONTEXT ( ( #26123 ) ) GLOBAL_UNIT_ASSIGNED_CONTEXT ( ( #24822, #26968, #22525 ) ) REPRESENTATION_CONTEXT ( 'NONE', 'WORKASPACE' ) );
#4038 = DIRECTION ( 'NONE',  ( 1.000000000000000000, -0.000000000000000000, 0.000000000000000000 ) ) ;
#4039 = DIRECTION ( 'NONE',  ( -0.000000000000000000, 0.000000000000000000, -1.000000000000000000 ) ) ;
#4040 = DIRECTION ( 'NONE',  ( 0.8916010070293584056, -0.4528218681382712996, 0.000000000000000000 ) ) ;
#4041 = VECTOR ( 'NONE', #25504, 1000.000000000000000 ) ;
#4042 = VERTEX_POINT ( 'NONE', #12827 ) ;
#4043 = CARTESIAN_POINT ( 'NONE',  ( -12.24491960465745599, 24.64876300893806160, 95.00000000000000000 ) ) ;
#4044 = AXIS2_PLACEMENT_3D ( 'NONE', #24192, #22178, #21891 ) ;
#4045 = CARTESIAN_POINT ( 'NONE',  ( -140.1213116003368668, 122.5384136796733827, 12.99999999999999822 ) ) ;
#4046 = PLANE ( 'NONE',  #17510 ) ;
#4047 = DIRECTION ( 'NONE',  ( -0.000000000000000000, 1.000000000000000000, -1.387778780781445429E-16 ) ) ;
#4048 = ORIENTED_EDGE ( 'NONE', *, *, #12709, .T. ) ;
#4049 = CARTESIAN_POINT ( 'NONE',  ( 157.4999999999994600, 213.7303124812313513, 45.00000000000000000 ) ) ;
#4050 = ADVANCED_FACE ( 'NONE', ( #25880 ), #11371, .F. ) ;
#4051 = DIRECTION ( 'NONE',  ( 0.8916010070293383105, -0.4528218681383106015, 0.000000000000000000 ) ) ;
#4052 = DIRECTION ( 'NONE',  ( 0.9506505318133482429, -0.3102637045530752258, 0.000000000000000000 ) ) ;
#4053 = CARTESIAN_POINT ( 'NONE',  ( -205.8189311304054172, 91.09162128824407034, 26.99035118652719589 ) ) ;
#4054 = VERTEX_POINT ( 'NONE', #10946 ) ;
#4055 =( NAMED_UNIT ( * ) SI_UNIT ( $, .STERADIAN. ) SOLID_ANGLE_UNIT ( ) );
#4056 = CARTESIAN_POINT ( 'NONE',  ( 502.4999999999996021, 44.41075299063185611, -75.35061095560293154 ) ) ;
#4057 = ORIENTED_EDGE ( 'NONE', *, *, #240, .F. ) ;
#4058 = LINE ( 'NONE', #12848, #3750 ) ;
#4059 = AXIS2_PLACEMENT_3D ( 'NONE', #21864, #2171, #10948 ) ;
#4060 = CARTESIAN_POINT ( 'NONE',  ( -178.8230272009045336, 110.7367001878539270, -29.27854200063107015 ) ) ;
#4061 = EDGE_LOOP ( 'NONE', ( #18002, #23361 ) ) ;
#4062 = ORIENTED_EDGE ( 'NONE', *, *, #13766, .T. ) ;
#4063 = LINE ( 'NONE', #26458, #24164 ) ;
#4064 = ORIENTED_EDGE ( 'NONE', *, *, #16923, .T. ) ;
#4065 = VECTOR ( 'NONE', #21116, 1000.000000000000114 ) ;
#4066 = ADVANCED_FACE ( 'NONE', ( #6911 ), #4461, .T. ) ;
#4067 = PRODUCT_DEFINITION_SHAPE ( 'NONE', 'NONE',  #25635 ) ;
#4068 = ADVANCED_FACE ( 'NONE', ( #317 ), #10909, .F. ) ;
#4069 = AXIS2_PLACEMENT_3D ( 'NONE', #7938, #8079, #25321 ) ;
#4070 = ORIENTED_EDGE ( 'NONE', *, *, #8217, .F. ) ;
#4071 = ORIENTED_EDGE ( 'NONE', *, *, #14135, .F. ) ;
#4072 = CARTESIAN_POINT ( 'NONE',  ( -68.57415822541635464, 75.97823757117562593, 100.0000000000000000 ) ) ;
#4073 = VECTOR ( 'NONE', #6904, 1000.000000000000000 ) ;
#4074 = DIRECTION ( 'NONE',  ( -1.000000000000000000, 0.000000000000000000, 0.000000000000000000 ) ) ;
#4075 = CARTESIAN_POINT ( 'NONE',  ( 232.4999999999996305, 133.0668745871126930, 36.86484227207694886 ) ) ;
#4076 = CARTESIAN_POINT ( 'NONE',  ( 158.0000000000000284, 205.9527499549551806, -45.00000000000000000 ) ) ;
#4077 = EDGE_CURVE ( 'NONE', #4843, #17557, #17612, .T. ) ;
#4078 = DIRECTION ( 'NONE',  ( -0.000000000000000000, 0.2756732917354685064, -0.9612513907525602752 ) ) ;
#4079 = DIRECTION ( 'NONE',  ( -0.000000000000000000, 1.000000000000000000, -1.387778780781445429E-16 ) ) ;
#4080 = CARTESIAN_POINT ( 'NONE',  ( -242.2202452114001971, 73.32912780460810609, -5.047888127322691432 ) ) ;
#4081 = VERTEX_POINT ( 'NONE', #17261 ) ;
#4082 = ADVANCED_FACE ( 'NONE', ( #6340 ), #15122, .F. ) ;
#4083 = AXIS2_PLACEMENT_3D ( 'NONE', #26593, #22151, #22005 ) ;
#4084 = CARTESIAN_POINT ( 'NONE',  ( 367.4999999999996021, 44.41075299063184900, 1.850330238640837654E-14 ) ) ;
#4085 = VECTOR ( 'NONE', #10734, 1000.000000000000000 ) ;
#4086 = CARTESIAN_POINT ( 'NONE',  ( 157.9999999999997158, 261.1260001201120531, 45.00000000000000000 ) ) ;
#4087 = DIRECTION ( 'NONE',  ( 0.000000000000000000, -1.000000000000000000, 0.000000000000000000 ) ) ;
#4088 = CARTESIAN_POINT ( 'NONE',  ( 113.0677398990926150, 225.0479495651688069, -97.20864094219261631 ) ) ;
#4089 = ORIENTED_EDGE ( 'NONE', *, *, #25864, .F. ) ;
#4090 = LINE ( 'NONE', #18900, #17827 ) ;
#4091 = VECTOR ( 'NONE', #5721, 1000.000000000000000 ) ;
#4092 = CARTESIAN_POINT ( 'NONE',  ( 167.4999999999996589, 494.4107529906318632, 84.99999999999995737 ) ) ;
#4093 = LINE ( 'NONE', #10997, #7349 ) ;
#4094 = CARTESIAN_POINT ( 'NONE',  ( 157.9999999999998295, 228.5236250225210313, -45.00000000000000000 ) ) ;
#4095 = CARTESIAN_POINT ( 'NONE',  ( 150.5563491861038870, 236.9705627484768797, 45.00000000000000000 ) ) ;
#4096 = CARTESIAN_POINT ( 'NONE',  ( 157.4999999999998579, 85.82868709837320864, 45.00000000000000000 ) ) ;
#4097 = VERTEX_POINT ( 'NONE', #5039 ) ;
#4098 = VECTOR ( 'NONE', #16114, 1000.000000000000227 ) ;
#4099 = DIRECTION ( 'NONE',  ( -0.4999999999999985012, 0.8660254037844394848, 0.000000000000000000 ) ) ;
#4100 = ORIENTED_EDGE ( 'NONE', *, *, #13426, .F. ) ;
#4101 = CARTESIAN_POINT ( 'NONE',  ( 65.00000000000000000, -170.0000000000000853, -69.99999999999998579 ) ) ;
#4102 = ORIENTED_EDGE ( 'NONE', *, *, #25165, .T. ) ;
#4103 = VERTEX_POINT ( 'NONE', #20271 ) ;
#4104 = CARTESIAN_POINT ( 'NONE',  ( 145.6339745962156940, 199.5814157129578064, -45.00000000000000000 ) ) ;
#4105 = EDGE_LOOP ( 'NONE', ( #25695, #5890, #24042, #26859 ) ) ;
#4106 = ADVANCED_FACE ( 'NONE', ( #22577 ), #876, .F. ) ;
#4107 = CIRCLE ( 'NONE', #16068, 21.20097097723064294 ) ;
#4108 = ORIENTED_EDGE ( 'NONE', *, *, #20852, .T. ) ;
#4109 = ORIENTED_EDGE ( 'NONE', *, *, #9554, .T. ) ;
#4110 = PLANE ( 'NONE',  #9070 ) ;
#4111 = CARTESIAN_POINT ( 'NONE',  ( -279.3160071107327553, -77.04550865309217045, 0.000000000000000000 ) ) ;
#4112 = DIRECTION ( 'NONE',  ( -0.000000000000000000, -0.000000000000000000, -1.000000000000000000 ) ) ;
#4113 = CARTESIAN_POINT ( 'NONE',  ( -160.0000000000000284, 119.7660240611718763, -22.85081902853004365 ) ) ;
#4114 = CARTESIAN_POINT ( 'NONE',  ( 158.0000000000004832, 163.3188748273380213, 45.00000000000000000 ) ) ;
#4115 = CARTESIAN_POINT ( 'NONE',  ( -262.5702831125496459, -171.5994388877033998, -94.99999999999987210 ) ) ;
#4116 = CARTESIAN_POINT ( 'NONE',  ( 20.31647538124909502, -48.17530653888324821, 98.86525827369392516 ) ) ;
#4117 = CARTESIAN_POINT ( 'NONE',  ( -218.7452477155994757, 87.82940237244157800, -19.01335168521931607 ) ) ;
#4118 = CARTESIAN_POINT ( 'NONE',  ( 131.9979426672184672, 249.8499243485765646, -139.8013169873307788 ) ) ;
#4119 = DIRECTION ( 'NONE',  ( -0.000000000000000000, -0.000000000000000000, -1.000000000000000000 ) ) ;
#4120 = DIRECTION ( 'NONE',  ( -0.000000000000000000, 0.000000000000000000, -1.000000000000000000 ) ) ;
#4121 = DIRECTION ( 'NONE',  ( -4.625929269271483942E-16, 1.000000000000000000, 0.000000000000000000 ) ) ;
#4122 = EDGE_CURVE ( 'NONE', #15118, #28119, #4993, .T. ) ;
#4123 = EDGE_LOOP ( 'NONE', ( #16163, #3080, #25060, #14868 ) ) ;
#4124 = EDGE_CURVE ( 'NONE', #27076, #2661, #15980, .T. ) ;
#4125 = AXIS2_PLACEMENT_3D ( 'NONE', #18888, #5679, #3654 ) ;
#4126 = LINE ( 'NONE', #1828, #456 ) ;
#4127 = DIRECTION ( 'NONE',  ( 0.000000000000000000, -1.000000000000000000, 0.000000000000000000 ) ) ;
#4128 = ADVANCED_FACE ( 'NONE', ( #26883 ), #18265, .F. ) ;
#4129 = CARTESIAN_POINT ( 'NONE',  ( -140.1240808061633345, 61.15703788601678781, -145.0000000000000000 ) ) ;
#4130 = ORIENTED_EDGE ( 'NONE', *, *, #8999, .F. ) ;
#4131 = VECTOR ( 'NONE', #18316, 999.9999999999998863 ) ;
#4132 = APPLICATION_CONTEXT ( 'automotive_design' ) ;
#4133 = CARTESIAN_POINT ( 'NONE',  ( 106.3805259670840258, 243.6561646000984922, -30.69292865457993713 ) ) ;
#4134 = EDGE_LOOP ( 'NONE', ( #23618, #19022, #185, #24923, #8663, #16702, #28248, #7472 ) ) ;
#4135 = CARTESIAN_POINT ( 'NONE',  ( -8.491711918032281758, 132.4972918898329226, -14.40622109717888755 ) ) ;
#4136 = ORIENTED_EDGE ( 'NONE', *, *, #18117, .T. ) ;
#4137 = ORIENTED_EDGE ( 'NONE', *, *, #9940, .F. ) ;
#4138 = ORIENTED_EDGE ( 'NONE', *, *, #22755, .T. ) ;
#4139 = ORIENTED_EDGE ( 'NONE', *, *, #19725, .F. ) ;
#4140 = ORIENTED_EDGE ( 'NONE', *, *, #23688, .F. ) ;
#4141 = DIRECTION ( 'NONE',  ( -0.000000000000000000, 0.000000000000000000, 1.000000000000000000 ) ) ;
#4142 = VECTOR ( 'NONE', #16154, 1000.000000000000000 ) ;
#4143 = B_SPLINE_CURVE_WITH_KNOTS ( 'NONE', 3,
 ( #28178, #8523, #17275, #3774, #12563, #4195, #16994, #21110, #8042, #1006, #14800, #16671, #23132, #10202, #5880, #9923, #18961, #10340, #20970, #25423, #23556, #8182 ),
 .UNSPECIFIED., .F., .F.,
 ( 4, 2, 2, 2, 2, 2, 2, 2, 2, 2, 4 ),
 ( 0.000000000000000000, 0.006853915506645740473, 0.01370783101329148095, 0.01713478876661434641, 0.02056174651993721014, 0.02741566202658293067, 0.03426957753322865119, 0.03769653528655152186, 0.04112349303987439253, 0.04797740854652013387, 0.05483132405316587521 ),
 .UNSPECIFIED. ) ;
#4144 = CARTESIAN_POINT ( 'NONE',  ( -412.2374841615667833, -120.0000000000002842, -100.0000000000000142 ) ) ;
#4145 = CARTESIAN_POINT ( 'NONE',  ( 167.4999999999996589, 526.4263741777961059, 84.99999999999995737 ) ) ;
#4146 = CARTESIAN_POINT ( 'NONE',  ( 147.3660254037845334, 200.5814157129577779, 45.00000000000000000 ) ) ;
#4147 = LINE ( 'NONE', #21831, #3423 ) ;
#4148 = ADVANCED_FACE ( 'NONE', ( #7206 ), #9647, .T. ) ;
#4149 = DIRECTION ( 'NONE',  ( 0.000000000000000000, -1.000000000000000000, 0.000000000000000000 ) ) ;
#4150 = CYLINDRICAL_SURFACE ( 'NONE', #20761, 5.999999999999991118 ) ;
#4151 = ADVANCED_FACE ( 'NONE', ( #27291 ), #16397, .F. ) ;
#4152 = CARTESIAN_POINT ( 'NONE',  ( 109.0192378864665557, 205.0000000000002842, -151.0000000000000284 ) ) ;
#4153 = ADVANCED_FACE ( 'NONE', ( #20688 ), #25142, .F. ) ;
#4154 = CYLINDRICAL_SURFACE ( 'NONE', #12825, 5.999999999999991118 ) ;
#4155 = CARTESIAN_POINT ( 'NONE',  ( -248.1546605714623013, -91.18033988749901653, 0.000000000000000000 ) ) ;
#4156 = DIRECTION ( 'NONE',  ( 0.8916010070298462376, 0.4528218681373109011, 0.000000000000000000 ) ) ;
#4158 = ORIENTED_EDGE ( 'NONE', *, *, #608, .F. ) ;
#4157 = ORIENTED_EDGE ( 'NONE', *, *, #14392, .T. ) ;
#4159 = CARTESIAN_POINT ( 'NONE',  ( -175.3965446499522045, 112.7547980845980646, 27.84039695627248889 ) ) ;
#4160=STYLED_ITEM('',(#28448),#18502);
#4161 = CARTESIAN_POINT ( 'NONE',  ( -270.6159714707433182, -170.3110992094025278, -103.8707009556082994 ) ) ;
#4162 = VERTEX_POINT ( 'NONE', #18544 ) ;
#4163 = ITEM_DEFINED_TRANSFORMATION ( 'NONE', 'NONE', #26707,  #10637 ) ;
#4164 = ORIENTED_EDGE ( 'NONE', *, *, #21247, .F. ) ;
#4165 = ORIENTED_EDGE ( 'NONE', *, *, #25110, .T. ) ;
#4166 = AXIS2_PLACEMENT_3D ( 'NONE', #13541, #19846, #5042 ) ;
#4167 = CARTESIAN_POINT ( 'NONE',  ( -215.4886702565632390, 139.8420026707766226, -13.00000000000000000 ) ) ;
#4168 = DIRECTION ( 'NONE',  ( 0.000000000000000000, 0.000000000000000000, -1.000000000000000000 ) ) ;
#4169 = ORIENTED_EDGE ( 'NONE', *, *, #11206, .F. ) ;
#4170 = ORIENTED_EDGE ( 'NONE', *, *, #21490, .T. ) ;
#4171 = CARTESIAN_POINT ( 'NONE',  ( 118.9718481642231609, 125.5986290015685398, -100.0000000000000142 ) ) ;
#4172 = LINE ( 'NONE', #24394, #23531 ) ;
#4173 = DIRECTION ( 'NONE',  ( 2.312964634635742464E-16, -1.000000000000000000, 0.000000000000000000 ) ) ;
#4174 = ORIENTED_EDGE ( 'NONE', *, *, #1814, .T. ) ;
#4175 = CARTESIAN_POINT ( 'NONE',  ( -228.1203047800660215, 90.71301417736495409, 13.39797158503563779 ) ) ;
#4176 = VERTEX_POINT ( 'NONE', #18404 ) ;
#4177 = CARTESIAN_POINT ( 'NONE',  ( 158.0000000000004547, 163.8267498348450886, 45.00000000000000000 ) ) ;
#4178 = EDGE_CURVE ( 'NONE', #25624, #4442, #741, .T. ) ;
#4179 = VECTOR ( 'NONE', #1090, 1000.000000000000114 ) ;
#4180 = FACE_OUTER_BOUND ( 'NONE', #9917, .T. ) ;
#4181 = CARTESIAN_POINT ( 'NONE',  ( 157.4999999999998579, 95.86018712840139244, 45.00000000000000000 ) ) ;
#4182 = VECTOR ( 'NONE', #791, 1000.000000000000000 ) ;
#4183 = EDGE_CURVE ( 'NONE', #14116, #11428, #27016, .T. ) ;
#4184 = DIRECTION ( 'NONE',  ( -0.000000000000000000, -1.000000000000000000, -0.000000000000000000 ) ) ;
#4185 = AXIS2_PLACEMENT_3D ( 'NONE', #10009, #16064, #22666 ) ;
#4186 = VERTEX_POINT ( 'NONE', #22720 ) ;
#4187 = CARTESIAN_POINT ( 'NONE',  ( 157.4999999999998579, 143.5098122710352015, 45.00000000000000000 ) ) ;
#4188 = ADVANCED_FACE ( 'NONE', ( #3023 ), #11810, .F. ) ;
#4189 = CARTESIAN_POINT ( 'NONE',  ( 157.4999999999997442, 256.3641876088515232, 45.00000000000000000 ) ) ;
#4190 = CARTESIAN_POINT ( 'NONE',  ( 158.0000000000007105, 136.2401247522676044, 45.00000000000000000 ) ) ;
#4191 = DIRECTION ( 'NONE',  ( -0.000000000000000000, -0.000000000000000000, -1.000000000000000000 ) ) ;
#4192 = ORIENTED_EDGE ( 'NONE', *, *, #16697, .T. ) ;
#4193 = DIRECTION ( 'NONE',  ( 1.000000000000000000, 0.000000000000000000, -0.000000000000000000 ) ) ;
#4194 = DIRECTION ( 'NONE',  ( 0.000000000000000000, 1.000000000000000000, 0.000000000000000000 ) ) ;
#4195 = CARTESIAN_POINT ( 'NONE',  ( -28.28141033279510808, 127.9583036527814386, -17.52276859028009071 ) ) ;
#4196 = CARTESIAN_POINT ( 'NONE',  ( -221.0638194754022265, 88.12640624682363466, 15.86102591047146682 ) ) ;
#4197 = ORIENTED_EDGE ( 'NONE', *, *, #10242, .T. ) ;
#4198 =( LENGTH_UNIT ( ) NAMED_UNIT ( * ) SI_UNIT ( .MILLI., .METRE. ) );
#4199 = LINE ( 'NONE', #18248, #13902 ) ;
#4200 = EDGE_LOOP ( 'NONE', ( #8700, #27746, #16871, #2025 ) ) ;
#4201 = VECTOR ( 'NONE', #20731, 1000.000000000000000 ) ;
#4202 = PLANE ( 'NONE',  #2836 ) ;
#4203 = CARTESIAN_POINT ( 'NONE',  ( -162.6948170962391487, 119.3828354928103579, -22.14444076542767448 ) ) ;
#4204 = ORIENTED_EDGE ( 'NONE', *, *, #18726, .F. ) ;
#4205 = AXIS2_PLACEMENT_3D ( 'NONE', #8103, #12289, #21447 ) ;
#4206 = PRODUCT_DEFINITION_FORMATION_WITH_SPECIFIED_SOURCE ( 'ANY', '', #4537, .NOT_KNOWN. ) ;
#4207 = ORIENTED_EDGE ( 'NONE', *, *, #4272, .F. ) ;
#4208 = FACE_OUTER_BOUND ( 'NONE', #12784, .T. ) ;
#4209 = ORIENTED_EDGE ( 'NONE', *, *, #17885, .F. ) ;
#4210 = COLOUR_RGB ( '',0.7921568627450980005, 0.8196078431372548767, 0.9333333333333333481 ) ;
#4211 = DIRECTION ( 'NONE',  ( -1.000000000000000000, -1.530283246943720875E-16, 0.000000000000000000 ) ) ;
#4213 = EDGE_CURVE ( 'NONE', #11481, #18743, #6304, .T. ) ;
#4212 = VERTEX_POINT ( 'NONE', #7494 ) ;
#4214 = ORIENTED_EDGE ( 'NONE', *, *, #28094, .T. ) ;
#4215 = CARTESIAN_POINT ( 'NONE',  ( 134.9999999999998579, 457.0747856552986832, -145.0000000000000000 ) ) ;
#4216 = EDGE_CURVE ( 'NONE', #22058, #6964, #16477, .T. ) ;
#4217 = LINE ( 'NONE', #10978, #3454 ) ;
#4218 = CARTESIAN_POINT ( 'NONE',  ( 157.4999999999998579, 98.36806213590843129, 45.00000000000000000 ) ) ;
#4219 = LINE ( 'NONE', #28337, #6670 ) ;
#4220 =( BOUNDED_CURVE ( )  B_SPLINE_CURVE ( 2, ( #23313, #19002, #12695 ),
 .UNSPECIFIED., .F., .F. ) 
 B_SPLINE_CURVE_WITH_KNOTS ( ( 3, 3 ),
 ( 0.000000000000000000, 1.000000000000000000 ),
 .UNSPECIFIED. ) 
 CURVE ( )  GEOMETRIC_REPRESENTATION_ITEM ( )  RATIONAL_B_SPLINE_CURVE ( ( 1.000000000000000000, 0.7071067811865475727, 1.000000000000000000 ) ) 
 REPRESENTATION_ITEM ( '' )  );
#4221 = CARTESIAN_POINT ( 'NONE',  ( 157.4999999999998579, 63.25781203080982351, 45.00000000000000000 ) ) ;
#4222 = DIRECTION ( 'NONE',  ( -1.000000000000000000, 0.000000000000000000, 0.000000000000000000 ) ) ;
#4223 = CARTESIAN_POINT ( 'NONE',  ( -244.5479615644635487, 75.99513337129094737, -15.00000000000000178 ) ) ;
#4224 = VERTEX_POINT ( 'NONE', #9789 ) ;
#4225 = AXIS2_PLACEMENT_3D ( 'NONE', #23564, #16540, #23144 ) ;
#4226 = CARTESIAN_POINT ( 'NONE',  ( 158.0000000000006537, 143.7637497747887210, 45.00000000000000000 ) ) ;
#4227 = EDGE_CURVE ( 'NONE', #27097, #17151, #458, .T. ) ;
#4228 = CARTESIAN_POINT ( 'NONE',  ( 158.0000000000014779, 65.51174953456337846, 45.00000000000000000 ) ) ;
#4230 = DIRECTION ( 'NONE',  ( -0.8916010070293783896, 0.4528218681382319422, 0.000000000000000000 ) ) ;
#4229 = AXIS2_PLACEMENT_3D ( 'NONE', #20054, #2812, #22216 ) ;
#4231 = ORIENTED_EDGE ( 'NONE', *, *, #7155, .F. ) ;
#4232 = CARTESIAN_POINT ( 'NONE',  ( 5.999999999999998224, 0.000000000000000000, 0.000000000000000000 ) ) ;
#4233 = CIRCLE ( 'NONE', #19841, 2.000000000000000000 ) ;
#4234 = EDGE_CURVE ( 'NONE', #19021, #6913, #2178, .T. ) ;
#4235 = DIRECTION ( 'NONE',  ( 0.000000000000000000, -1.000000000000000000, 0.000000000000000000 ) ) ;
#4236 = FACE_OUTER_BOUND ( 'NONE', #9986, .T. ) ;
#4237 = CARTESIAN_POINT ( 'NONE',  ( 158.0000000000007958, 128.7164997297464595, 45.00000000000000000 ) ) ;
#4238 = CARTESIAN_POINT ( 'NONE',  ( 109.9999999999999147, 140.0000000000000000, 90.00000000000002842 ) ) ;
#4239 = DIRECTION ( 'NONE',  ( -0.000000000000000000, -0.000000000000000000, -1.000000000000000000 ) ) ;
#4240 = ORIENTED_EDGE ( 'NONE', *, *, #22065, .F. ) ;
#4241 = LINE ( 'NONE', #25649, #21237 ) ;
#4242 = EDGE_LOOP ( 'NONE', ( #26927, #2909, #13178, #28392 ) ) ;
#4243 = CARTESIAN_POINT ( 'NONE',  ( 157.4999999999998579, 181.1279373836408411, -45.00000000000000000 ) ) ;
#4244 = ORIENTED_EDGE ( 'NONE', *, *, #13892, .F. ) ;
#4245 = EDGE_CURVE ( 'NONE', #20893, #3887, #24585, .T. ) ;
#4246 = VECTOR ( 'NONE', #12334, 1000.000000000000114 ) ;
#4247 = ORIENTED_EDGE ( 'NONE', *, *, #3106, .F. ) ;
#4248 = LINE ( 'NONE', #23938, #7166 ) ;
#4249 = VECTOR ( 'NONE', #28071, 1000.000000000000114 ) ;
#4250 = EDGE_LOOP ( 'NONE', ( #17899, #27, #24146, #6205 ) ) ;
#4251 = VERTEX_POINT ( 'NONE', #14381 ) ;
#4252 = AXIS2_PLACEMENT_3D ( 'NONE', #8758, #15519, #15233 ) ;
#4253 = CARTESIAN_POINT ( 'NONE',  ( -222.2072112174627136, 138.1987073436359026, 14.97424725141359403 ) ) ;
#4254 = DIRECTION ( 'NONE',  ( 0.000000000000000000, 0.000000000000000000, 1.000000000000000000 ) ) ;
#4255 = CARTESIAN_POINT ( 'NONE',  ( -210.4359063544880541, -219.8547609215023328, 91.14353391724667119 ) ) ;
#4256 = VECTOR ( 'NONE', #4517, 1000.000000000000000 ) ;
#4257 = EDGE_CURVE ( 'NONE', #21319, #8486, #23559, .T. ) ;
#4258 = LINE ( 'NONE', #21791, #27727 ) ;
#4259 = CARTESIAN_POINT ( 'NONE',  ( 157.4999999999997442, 253.8563126013445697, 45.00000000000000000 ) ) ;
#4260 = CARTESIAN_POINT ( 'NONE',  ( 158.0000000000017337, 42.94087446699998623, 45.00000000000000000 ) ) ;
#4261 = CARTESIAN_POINT ( 'NONE',  ( -210.0000000000000568, -152.0000000000000284, -110.0000000000000284 ) ) ;
#4262 = CARTESIAN_POINT ( 'NONE',  ( -218.2708698084869638, 86.23473497505111141, -19.67429589792924816 ) ) ;
#4263 = DIRECTION ( 'NONE',  ( -0.000000000000000000, -0.000000000000000000, -1.000000000000000000 ) ) ;
#4264 = CARTESIAN_POINT ( 'NONE',  ( -260.0000000000001137, -152.0000000000000284, -59.99999999999986500 ) ) ;
#4265 = FACE_OUTER_BOUND ( 'NONE', #6382, .T. ) ;
#4266 = CARTESIAN_POINT ( 'NONE',  ( 372.9108539694884144, -280.0000000000000568, 167.7200181511720132 ) ) ;
#4267 = LINE ( 'NONE', #17059, #24938 ) ;
#4268 = ORIENTED_EDGE ( 'NONE', *, *, #17273, .F. ) ;
#4269 = AXIS2_PLACEMENT_3D ( 'NONE', #18991, #12687, #5774 ) ;
#4270 = CARTESIAN_POINT ( 'NONE',  ( 179.9999999999999147, 526.4263741777961059, -100.0000000000000142 ) ) ;
#4271 = ADVANCED_FACE ( 'NONE', ( #10206 ), #23276, .F. ) ;
#4272 = EDGE_CURVE ( 'NONE', #18330, #12180, #18818, .T. ) ;
#4273 = VECTOR ( 'NONE', #24918, 1000.000000000000000 ) ;
#4274 = CARTESIAN_POINT ( 'NONE',  ( 186.0596930950812293, 94.49506802741289846, 45.00000000000000000 ) ) ;
#4275 = DIRECTION ( 'NONE',  ( 0.8916010070299679180, 0.4528218681370710930, 0.000000000000000000 ) ) ;
#4276 = CARTESIAN_POINT ( 'NONE',  ( 106.5565118542854322, 210.4619613463102894, -145.7848141779619198 ) ) ;
#4277 = AXIS2_PLACEMENT_3D ( 'NONE', #2108, #4121, #23959 ) ;
#4278 = ORIENTED_EDGE ( 'NONE', *, *, #14915, .F. ) ;
#4279 = CARTESIAN_POINT ( 'NONE',  ( 93.26488863019004327, 240.2518291191186393, -7.855680688305695547 ) ) ;
#4280 = ORIENTED_EDGE ( 'NONE', *, *, #17709, .F. ) ;
#4281 = LINE ( 'NONE', #403, #10536 ) ;
#4282 = ORIENTED_EDGE ( 'NONE', *, *, #14945, .F. ) ;
#4283 = ADVANCED_FACE ( 'NONE', ( #5606 ), #12659, .F. ) ;
#4284 = EDGE_LOOP ( 'NONE', ( #500, #10010, #26500, #14827 ) ) ;
#4285 = ORIENTED_EDGE ( 'NONE', *, *, #2794, .T. ) ;
#4286 = ORIENTED_EDGE ( 'NONE', *, *, #7759, .F. ) ;
#4287 = VERTEX_POINT ( 'NONE', #12374 ) ;
#4288 = AXIS2_PLACEMENT_3D ( 'NONE', #15263, #8927, #22138 ) ;
#4289 = DIRECTION ( 'NONE',  ( 1.000000000000000000, 0.000000000000000000, 0.000000000000000000 ) ) ;
#4290 = EDGE_CURVE ( 'NONE', #2965, #18534, #1293, .T. ) ;
#4291 = VECTOR ( 'NONE', #4351, 1000.000000000000000 ) ;
#4292 = CARTESIAN_POINT ( 'NONE',  ( -107.3221550338875687, 17.24192588826928585, 80.00000000000001421 ) ) ;
#4293 = ADVANCED_FACE ( 'NONE', ( #21255, #14245, #12511, #7902, #16673 ), #3443, .T. ) ;
#4294 = AXIS2_PLACEMENT_3D ( 'NONE', #24629, #6806, #15451 ) ;
#4295 = UNCERTAINTY_MEASURE_WITH_UNIT (LENGTH_MEASURE( 1.000000000000000082E-05 ), #4198, 'distance_accuracy_value', 'NONE');
#4296 = CARTESIAN_POINT ( 'NONE',  ( -175.0000000000000000, -150.0000000000000853, -64.00000000000000000 ) ) ;
#4297 = FACE_OUTER_BOUND ( 'NONE', #25874, .T. ) ;
#4298 = CARTESIAN_POINT ( 'NONE',  ( -119.0030847931093518, 214.2064521616283059, -5.000000000000004441 ) ) ;
#4299 = CYLINDRICAL_SURFACE ( 'NONE', #26365, 16.07743405327025243 ) ;
#4300 = PLANE ( 'NONE',  #12768 ) ;
#4301 = CARTESIAN_POINT ( 'NONE',  ( -189.8086322075389774, 92.49158130768422836, 15.00000000000000000 ) ) ;
#4302 = DIRECTION ( 'NONE',  ( 0.000000000000000000, 1.000000000000000000, 0.000000000000000000 ) ) ;
#4303 = FACE_OUTER_BOUND ( 'NONE', #21706, .T. ) ;
#4304 = LINE ( 'NONE', #16956, #14750 ) ;
#4305 = CARTESIAN_POINT ( 'NONE',  ( 65.00000000000000000, -120.0000000000000711, 70.00000000000001421 ) ) ;
#4307 = EDGE_LOOP ( 'NONE', ( #22135, #22842, #7042, #20194 ) ) ;
#4306 = ORIENTED_EDGE ( 'NONE', *, *, #13602, .T. ) ;
#4308 = VECTOR ( 'NONE', #22175, 1000.000000000000000 ) ;
#4309 = CARTESIAN_POINT ( 'NONE',  ( -167.4985236603498038, 116.4129322153221437, 25.86027712211474494 ) ) ;
#4310 = CARTESIAN_POINT ( 'NONE',  ( 157.9999999999997158, 261.1260001201120531, 45.00000000000000000 ) ) ;
#4311 = EDGE_LOOP ( 'NONE', ( #15283, #10947, #2895, #12145 ) ) ;
#4312 = VECTOR ( 'NONE', #26313, 1000.000000000000227 ) ;
#4313 = ORIENTED_EDGE ( 'NONE', *, *, #23337, .T. ) ;
#4314 = VERTEX_POINT ( 'NONE', #16811 ) ;
#4315 = DIRECTION ( 'NONE',  ( 1.000000000000000000, 0.000000000000000000, 0.000000000000000000 ) ) ;
#4316 = CARTESIAN_POINT ( 'NONE',  ( 209.9999999999999432, -150.0000000000000284, 99.99999999999991473 ) ) ;
#4317 = ORIENTED_EDGE ( 'NONE', *, *, #6465, .T. ) ;
#4318 = CARTESIAN_POINT ( 'NONE',  ( 119.9999999987673220, 136.1131920016294714, -100.0000000000000142 ) ) ;
#4319 = EDGE_CURVE ( 'NONE', #14508, #3426, #22993, .T. ) ;
#4320 = CARTESIAN_POINT ( 'NONE',  ( 93.99999999999985789, 268.4896896257338312, 84.99999999999995737 ) ) ;
#4321 = VERTEX_POINT ( 'NONE', #25284 ) ;
#4322 = CARTESIAN_POINT ( 'NONE',  ( -221.9429674677837170, 88.28884742766322802, 17.46146441898723722 ) ) ;
#4323 = ORIENTED_EDGE ( 'NONE', *, *, #19214, .T. ) ;
#4324 = CARTESIAN_POINT ( 'NONE',  ( -175.0000000000000000, -150.0000000000000853, 70.00000000000001421 ) ) ;
#4325 = FACE_OUTER_BOUND ( 'NONE', #11853, .T. ) ;
#4326 = CIRCLE ( 'NONE', #24074, 6.000000000000005329 ) ;
#4327 = CARTESIAN_POINT ( 'NONE',  ( 159.3470388241378259, 202.4691944533894912, -150.2059422892478722 ) ) ;
#4328 = DIRECTION ( 'NONE',  ( 1.000000000000000000, -0.000000000000000000, -0.000000000000000000 ) ) ;
#4329 = VERTEX_POINT ( 'NONE', #3580 ) ;
#4330 = DIRECTION ( 'NONE',  ( 0.8916010070293584056, 0.4528218681382713551, 0.000000000000000000 ) ) ;
#4331 = ADVANCED_FACE ( 'NONE', ( #14521 ), #21113, .F. ) ;
#4332 = DIRECTION ( 'NONE',  ( 0.000000000000000000, 0.000000000000000000, -1.000000000000000000 ) ) ;
#4333 = LINE ( 'NONE', #17694, #6953 ) ;
#4334 = CARTESIAN_POINT ( 'NONE',  ( 157.9999999999998579, 221.5078750075070104, -45.00000000000000000 ) ) ;
#4335 = ORIENTED_EDGE ( 'NONE', *, *, #16804, .F. ) ;
#4336 = DIRECTION ( 'NONE',  ( 0.000000000000000000, 0.000000000000000000, 1.000000000000000000 ) ) ;
#4337 = ADVANCED_FACE ( 'NONE', ( #23412 ), #1576, .F. ) ;
#4338 = DIRECTION ( 'NONE',  ( -0.000000000000000000, -0.000000000000000000, -1.000000000000000000 ) ) ;
#4339 = CARTESIAN_POINT ( 'NONE',  ( -213.5112655984951857, 88.12920823218718169, 20.63189810804927049 ) ) ;
#4340 = VERTEX_POINT ( 'NONE', #27844 ) ;
#4341 = ORIENTED_EDGE ( 'NONE', *, *, #386, .T. ) ;
#4342 = VECTOR ( 'NONE', #26882, 1000.000000000000114 ) ;
#4343 = LINE ( 'NONE', #6359, #17050 ) ;
#4344 = CARTESIAN_POINT ( 'NONE',  ( -184.0646120581192520, 107.4357226780370667, -31.54942295155680654 ) ) ;
#4345 = VERTEX_POINT ( 'NONE', #16950 ) ;
#4346 = ADVANCED_FACE ( 'NONE', ( #25704 ), #6025, .F. ) ;
#4347 = CONICAL_SURFACE ( 'NONE', #11258, 6.025000000000002132, 0.7853981633974482790 ) ;
#4348 = ORIENTED_EDGE ( 'NONE', *, *, #9095, .T. ) ;
#4349 = EDGE_CURVE ( 'NONE', #5984, #15146, #24737, .T. ) ;
#4350 = DIRECTION ( 'NONE',  ( 1.000000000000000000, 0.000000000000000000, -0.000000000000000000 ) ) ;
#4351 = DIRECTION ( 'NONE',  ( -0.000000000000000000, -1.000000000000000000, -0.000000000000000000 ) ) ;
#4352 = EDGE_CURVE ( 'NONE', #24036, #6606, #19245, .T. ) ;
#4353 = ORIENTED_EDGE ( 'NONE', *, *, #26551, .T. ) ;
#4354 = EDGE_LOOP ( 'NONE', ( #10832, #19485, #5666, #12241 ) ) ;
#4355 = DIRECTION ( 'NONE',  ( -0.8660254037844363761, 0.5000000000000039968, -0.000000000000000000 ) ) ;
#4356 = FACE_OUTER_BOUND ( 'NONE', #18639, .T. ) ;
#4357 = VECTOR ( 'NONE', #15478, 999.9999999999998863 ) ;
#4358 = DIRECTION ( 'NONE',  ( -0.000000000000000000, -0.000000000000000000, -1.000000000000000000 ) ) ;
#4359 = DIRECTION ( 'NONE',  ( -0.000000000000000000, -0.000000000000000000, -1.000000000000000000 ) ) ;
#4360 = DIRECTION ( 'NONE',  ( -0.8916010070297041290, -0.4528218681375906218, 0.000000000000000000 ) ) ;
#4361 = AXIS2_PLACEMENT_3D ( 'NONE', #24230, #11163, #26511 ) ;
#4362 = CARTESIAN_POINT ( 'NONE',  ( -209.9870472515087840, 61.15599310541787048, -23.95647182577626921 ) ) ;
#4363 = DIRECTION ( 'NONE',  ( -0.000000000000000000, -0.000000000000000000, -1.000000000000000000 ) ) ;
#4364 = ORIENTED_EDGE ( 'NONE', *, *, #26079, .T. ) ;
#4365 = DIRECTION ( 'NONE',  ( -0.8916010070293383105, -0.4528218681383106015, 0.000000000000000000 ) ) ;
#4366 = VECTOR ( 'NONE', #19997, 1000.000000000000000 ) ;
#4367 = DIRECTION ( 'NONE',  ( 0.000000000000000000, -1.000000000000000000, 0.000000000000000000 ) ) ;
#4368 = FACE_OUTER_BOUND ( 'NONE', #3397, .T. ) ;
#4369 = CARTESIAN_POINT ( 'NONE',  ( 157.9999999999996589, 271.6653751576470768, 45.00000000000000000 ) ) ;
#4370 = ORIENTED_EDGE ( 'NONE', *, *, #10270, .F. ) ;
#4371 = LINE ( 'NONE', #24487, #25190 ) ;
#4372 = DIRECTION ( 'NONE',  ( 1.000000000000000000, 0.000000000000000000, 0.000000000000000000 ) ) ;
#4373 = DIRECTION ( 'NONE',  ( 0.4528218681380514754, 0.8916010070294700940, -0.000000000000000000 ) ) ;
#4374 = CYLINDRICAL_SURFACE ( 'NONE', #3898, 2.586968381275096984 ) ;
#4375 = LINE ( 'NONE', #6396, #24854 ) ;
#4376 = CARTESIAN_POINT ( 'NONE',  ( -180.0000000000000284, 59.99999999999994316, -100.0000000000000142 ) ) ;
#4377 = EDGE_LOOP ( 'NONE', ( #16558, #1093 ) ) ;
#4378 = ADVANCED_FACE ( 'NONE', ( #5461 ), #3298, .F. ) ;
#4379 = CARTESIAN_POINT ( 'NONE',  ( -207.5044420441007560, 75.59897387903042443, 45.00000000000000000 ) ) ;
#4380 = ORIENTED_EDGE ( 'NONE', *, *, #11326, .T. ) ;
#4381 = CARTESIAN_POINT ( 'NONE',  ( -270.7820719900048516, -170.3051706208958365, 93.45761744549247396 ) ) ;
#4382 = ORIENTED_EDGE ( 'NONE', *, *, #19112, .T. ) ;
#4383 = CIRCLE ( 'NONE', #11759, 17.93072811908088937 ) ;
#4384 = VECTOR ( 'NONE', #3375, 1000.000000000000000 ) ;
#4385 = CIRCLE ( 'NONE', #20452, 30.00000000000002842 ) ;
#4386 = ORIENTED_EDGE ( 'NONE', *, *, #9623, .F. ) ;
#4387 = PLANE ( 'NONE',  #10378 ) ;
#4388 = EDGE_CURVE ( 'NONE', #22451, #3081, #1998, .T. ) ;
#4389 = VERTEX_POINT ( 'NONE', #14948 ) ;
#4390 =( BOUNDED_SURFACE ( )  B_SPLINE_SURFACE ( 3, 2, ( 
 ( #9631, #2118, #17069 ),
 ( #6009, #12916, #28387 ),
 ( #19226, #26107, #28257 ),
 ( #4279, #23967, #10895 ),
 ( #1978, #17213, #6437 ),
 ( #25830, #12639, #1697 ),
 ( #21380, #25972, #12777 ),
 ( #23683, #19650, #10468 ),
 ( #21520, #17347, #27971 ),
 ( #19512, #8315, #10755 ),
 ( #15213, #13065, #6156 ),
 ( #8735, #25688, #14929 ),
 ( #10609, #14784, #3988 ),
 ( #21811, #1559, #14641 ),
 ( #17488, #5864, #23395 ),
 ( #3703, #12494, #6288 ),
 ( #15066, #21238, #23542 ),
 ( #3851, #1834, #19366 ),
 ( #10325, #27829, #28116 ),
 ( #8457, #23825, #4133 ),
 ( #21663, #8167, #8597 ),
 ( #19087, #16931, #15639 ),
 ( #21945, #24243, #26525 ),
 ( #22087, #544, #17921 ),
 ( #9309, #11622, #11178 ),
 ( #4415, #6856, #2827 ),
 ( #4693, #18072, #11475 ),
 ( #15786, #24529, #2254 ),
 ( #15357, #22523, #4839 ),
 ( #20364, #9021, #9457 ) ),
 .UNSPECIFIED., .F., .F., .F. ) 
 B_SPLINE_SURFACE_WITH_KNOTS ( ( 4, 2, 2, 2, 2, 2, 2, 2, 2, 2, 2, 2, 2, 2, 4 ),
 ( 3, 3 ),
 ( 0.000000000000000000, 0.003854887539719038109, 0.007709775079438076217, 0.009637218849297595272, 0.01156466261915711433, 0.01541955015887615243, 0.01927443769859519054, 0.02312932523831422865, 0.03083910031775230487, 0.03469398785747133951, 0.03854887539719038109, 0.04625865047662845730, 0.05396842555606653352, 0.05782331309578557510, 0.06167820063550460974 ),
 ( 0.000000000000000000, 1.000000000000000000 ),
 .UNSPECIFIED. ) 
 GEOMETRIC_REPRESENTATION_ITEM ( )  RATIONAL_B_SPLINE_SURFACE ( (
 ( 1.000000000000000000, 0.7071067811865491270, 1.000000000000000000),
 ( 1.000000000000000000, 0.7108376764369856993, 1.000000000000000000),
 ( 1.000000000000000000, 0.7158505121285758666, 1.000000000000000000),
 ( 1.000000000000000000, 0.7278978148825536731, 1.000000000000000000),
 ( 1.000000000000000000, 0.7349313210304360133, 1.000000000000000000),
 ( 1.000000000000000000, 0.7466216138177209638, 1.000000000000000000),
 ( 1.000000000000000000, 0.7507087799372132997, 1.000000000000000000),
 ( 1.000000000000000000, 0.7592063458283927480, 1.000000000000000000),
 ( 1.000000000000000000, 0.7635836989921321871, 1.000000000000000000),
 ( 1.000000000000000000, 0.7769550404251118758, 1.000000000000000000),
 ( 1.000000000000000000, 0.7862062597111377782, 1.000000000000000000),
 ( 1.000000000000000000, 0.8049739164093935306, 1.000000000000000000),
 ( 1.000000000000000000, 0.8144916847802230464, 1.000000000000000000),
 ( 1.000000000000000000, 0.8334855532645426557, 1.000000000000000000),
 ( 1.000000000000000000, 0.8428380035006605153, 1.000000000000000000),
 ( 1.000000000000000000, 0.8700856926957447612, 1.000000000000000000),
 ( 1.000000000000000000, 0.8872021369645698430, 1.000000000000000000),
 ( 1.000000000000000000, 0.9106340391013421076, 1.000000000000000000),
 ( 1.000000000000000000, 0.9180764524644583480, 1.000000000000000000),
 ( 1.000000000000000000, 0.9321377268945353345, 1.000000000000000000),
 ( 1.000000000000000000, 0.9386792981684866088, 1.000000000000000000),
 ( 1.000000000000000000, 0.9568359836574985566, 1.000000000000000000),
 ( 1.000000000000000000, 0.9669855263606685902, 1.000000000000000000),
 ( 1.000000000000000000, 0.9833405099237995106, 1.000000000000000000),
 ( 1.000000000000000000, 0.9895476861107730393, 1.000000000000000000),
 ( 1.000000000000000000, 0.9958061391666522821, 1.000000000000000000),
 ( 1.000000000000000000, 0.9973811977640341109, 1.000000000000000000),
 ( 1.000000000000000000, 0.9994757700714922422, 1.000000000000000000),
 ( 1.000000000000000000, 1.000000000000000000, 1.000000000000000000),
 ( 1.000000000000000000, 1.000000000000000000, 1.000000000000000000) ) ) 
 REPRESENTATION_ITEM ( '' )  SURFACE ( )  );
#4391 = AXIS2_PLACEMENT_3D ( 'NONE', #4538, #13051, #11162 ) ;
#4392 = VERTEX_POINT ( 'NONE', #11201 ) ;
#4393 = FACE_OUTER_BOUND ( 'NONE', #2591, .T. ) ;
#4394 = CARTESIAN_POINT ( 'NONE',  ( 89.77759941121971110, 81.13568025368125802, 100.0000000000000142 ) ) ;
#4395 = CARTESIAN_POINT ( 'NONE',  ( 106.7826897485233815, 249.1041097334432948, 25.92390487273943123 ) ) ;
#4396 = LINE ( 'NONE', #24224, #25465 ) ;
#4397 = PLANE ( 'NONE',  #27493 ) ;
#4398 = CARTESIAN_POINT ( 'NONE',  ( 217.4999999999996305, 133.0668745871126930, 42.86484227207692044 ) ) ;
#4399 = LINE ( 'NONE', #26236, #714 ) ;
#4400 = CARTESIAN_POINT ( 'NONE',  ( -210.7172313291012529, 103.7585653882801182, 15.00000000000000000 ) ) ;
#4401 = PLANE ( 'NONE',  #19570 ) ;
#4402 = CARTESIAN_POINT ( 'NONE',  ( 157.4999999999998579, 55.73418700828869277, 45.00000000000000000 ) ) ;
#4403 = PLANE ( 'NONE',  #26656 ) ;
#4404 = CARTESIAN_POINT ( 'NONE',  ( 157.9999999999998295, 226.0157500150140208, 45.00000000000000000 ) ) ;
#4405 = LINE ( 'NONE', #21507, #26296 ) ;
#4406 = AXIS2_PLACEMENT_3D ( 'NONE', #2368, #231, #15609 ) ;
#4407 = VERTEX_POINT ( 'NONE', #136 ) ;
#4408 = LINE ( 'NONE', #20061, #24819 ) ;
#4409 = DIRECTION ( 'NONE',  ( -0.000000000000000000, 0.000000000000000000, 1.000000000000000000 ) ) ;
#4410 = DIRECTION ( 'NONE',  ( -1.000000000000000000, 0.000000000000000000, 0.000000000000000000 ) ) ;
#4411 = CARTESIAN_POINT ( 'NONE',  ( -68.97958094182604327, 102.2323340340523288, -145.0000000000000000 ) ) ;
#4412 = AXIS2_PLACEMENT_3D ( 'NONE', #6565, #19497, #24098 ) ;
#4413 = VERTEX_POINT ( 'NONE', #2418 ) ;
#4414 = EDGE_CURVE ( 'NONE', #21067, #8004, #9544, .T. ) ;
#4415 = CARTESIAN_POINT ( 'NONE',  ( 109.8079904624971590, 257.1776683528169656, -40.10892953523403293 ) ) ;
#4416 = ORIENTED_EDGE ( 'NONE', *, *, #6558, .T. ) ;
#4417 = CARTESIAN_POINT ( 'NONE',  ( 158.0000000000012790, 83.57474959461971764, 45.00000000000000000 ) ) ;
#4418 = ORIENTED_EDGE ( 'NONE', *, *, #17562, .T. ) ;
#4419 = ORIENTED_EDGE ( 'NONE', *, *, #26008, .F. ) ;
#4420 = VERTEX_POINT ( 'NONE', #15232 ) ;
#4421 = ORIENTED_EDGE ( 'NONE', *, *, #21725, .T. ) ;
#4422 = CARTESIAN_POINT ( 'NONE',  ( 134.9999999999998579, 467.1080826427131001, -145.0000000000000000 ) ) ;
#4423 = CIRCLE ( 'NONE', #1679, 7.499999999999992895 ) ;
#4424 = CARTESIAN_POINT ( 'NONE',  ( 124.3660254037843771, 240.4185842870417105, -45.00000000000000000 ) ) ;
#4425 = EDGE_CURVE ( 'NONE', #11428, #13449, #287, .T. ) ;
#4426 = EDGE_CURVE ( 'NONE', #9458, #11694, #17657, .T. ) ;
#4427 = LINE ( 'NONE', #8890, #5944 ) ;
#4428 = FACE_OUTER_BOUND ( 'NONE', #14961, .T. ) ;
#4429 = CARTESIAN_POINT ( 'NONE',  ( -215.5934637701523684, 59.01440814108518396, 29.65465734991407132 ) ) ;
#4430 = DIRECTION ( 'NONE',  ( 0.000000000000000000, -1.000000000000000000, -1.214306433183764966E-16 ) ) ;
#4431 = FACE_OUTER_BOUND ( 'NONE', #7617, .T. ) ;
#4432 = CARTESIAN_POINT ( 'NONE',  ( -68.57415822541635464, 29.64876300893806516, 100.0000000000000000 ) ) ;
#4433 = FACE_OUTER_BOUND ( 'NONE', #5415, .T. ) ;
#4434 = DIRECTION ( 'NONE',  ( 0.000000000000000000, -1.000000000000000000, 0.000000000000000000 ) ) ;
#4435 = DIRECTION ( 'NONE',  ( 1.000000000000000000, -0.000000000000000000, -0.000000000000000000 ) ) ;
#4436 = EDGE_CURVE ( 'NONE', #8166, #4103, #9043, .T. ) ;
#4437 = ADVANCED_FACE ( 'NONE', ( #26411 ), #21832, .F. ) ;
#4438 = CARTESIAN_POINT ( 'NONE',  ( -33.80003448231774854, 129.4040373687968497, 16.90087253816493273 ) ) ;
#4439 = CARTESIAN_POINT ( 'NONE',  ( 0.000000000000000000, -1.249999999999999112, -6.997769477110050929 ) ) ;
#4440 = DIRECTION ( 'NONE',  ( 1.530283246943720875E-16, -1.000000000000000000, 0.000000000000000000 ) ) ;
#4441 = DIRECTION ( 'NONE',  ( 1.000000000000000000, -0.000000000000000000, -0.000000000000000000 ) ) ;
#4443 = ORIENTED_EDGE ( 'NONE', *, *, #17601, .F. ) ;
#4442 = VERTEX_POINT ( 'NONE', #6171 ) ;
#4444 = VECTOR ( 'NONE', #14125, 1000.000000000000000 ) ;
#4445 = CARTESIAN_POINT ( 'NONE',  ( -229.9492672981298824, 89.43170946566928592, -15.28058751945465410 ) ) ;
#4446 = CARTESIAN_POINT ( 'NONE',  ( -210.0000000000000568, -160.0000000000001421, 110.0000000000000284 ) ) ;
#4447 = ORIENTED_EDGE ( 'NONE', *, *, #16149, .F. ) ;
#4448 = EDGE_CURVE ( 'NONE', #20275, #1752, #28332, .T. ) ;
#4449 = EDGE_LOOP ( 'NONE', ( #6153, #27694, #15526, #26157 ) ) ;
#4450 = ORIENTED_EDGE ( 'NONE', *, *, #24237, .F. ) ;
#4451 = DIRECTION ( 'NONE',  ( -0.8916010070297542001, 0.4528218681374919785, 0.000000000000000000 ) ) ;
#4452 = DIRECTION ( 'NONE',  ( -0.8916010070293283185, -0.4528218681383305855, 0.000000000000000000 ) ) ;
#4453 = ORIENTED_EDGE ( 'NONE', *, *, #7211, .F. ) ;
#4454 = CARTESIAN_POINT ( 'NONE',  ( 117.1152841538456926, 116.0550883417529491, -100.0000000000000142 ) ) ;
#4455 = CARTESIAN_POINT ( 'NONE',  ( 158.0000000000003411, 173.8582498648732440, 45.00000000000000000 ) ) ;
#4456 = ORIENTED_EDGE ( 'NONE', *, *, #12321, .T. ) ;
#4457 = CARTESIAN_POINT ( 'NONE',  ( -218.7796873555838033, 87.80254006751567886, 18.97549214882609903 ) ) ;
#4458 = CIRCLE ( 'NONE', #14573, 5.999999999999977796 ) ;
#4459 = LINE ( 'NONE', #19982, #1074 ) ;
#4460 = FACE_OUTER_BOUND ( 'NONE', #22710, .T. ) ;
#4461 = PLANE ( 'NONE',  #13741 ) ;
#4462 = ORIENTED_EDGE ( 'NONE', *, *, #6713, .F. ) ;
#4463 = FACE_OUTER_BOUND ( 'NONE', #3499, .T. ) ;
#4464 = CARTESIAN_POINT ( 'NONE',  ( -225.3736415174480214, 135.7651958811098325, -14.97905406095859959 ) ) ;
#4465 = DIRECTION ( 'NONE',  ( 0.000000000000000000, 0.000000000000000000, -1.000000000000000000 ) ) ;
#4466 = CARTESIAN_POINT ( 'NONE',  ( -235.6837214056122036, 120.7228219557777180, -13.00000000000000000 ) ) ;
#4467 = ORIENTED_EDGE ( 'NONE', *, *, #4257, .F. ) ;
#4468 = ADVANCED_FACE ( 'NONE', ( #23701 ), #4300, .F. ) ;
#4469 = DIRECTION ( 'NONE',  ( 1.000000000000000000, 0.000000000000000000, -0.000000000000000000 ) ) ;
#4470 = EDGE_CURVE ( 'NONE', #20648, #6227, #15514, .T. ) ;
#4471 = AXIS2_PLACEMENT_3D ( 'NONE', #19534, #2138, #6734 ) ;
#4472 = CARTESIAN_POINT ( 'NONE',  ( 145.9999999999998863, 220.0000000000000284, 99.00000000000001421 ) ) ;
#4473 = DIRECTION ( 'NONE',  ( -0.000000000000000000, 1.000000000000000000, -1.387778780781445429E-16 ) ) ;
#4474 = ORIENTED_EDGE ( 'NONE', *, *, #21612, .F. ) ;
#4475 = ADVANCED_FACE ( 'NONE', ( #13361 ), #24265, .F. ) ;
#4476 = ORIENTED_EDGE ( 'NONE', *, *, #13852, .F. ) ;
#4477 = DIRECTION ( 'NONE',  ( -0.5457381880580697286, 0.8379557447115539848, 0.000000000000000000 ) ) ;
#4478 = CARTESIAN_POINT ( 'NONE',  ( -180.2001402660981455, 109.5948180456561261, -30.90938774632539321 ) ) ;
#4479 = VERTEX_POINT ( 'NONE', #12934 ) ;
#4480 = EDGE_LOOP ( 'NONE', ( #1026, #25485, #16593, #3220, #23899, #183, #955, #22157 ) ) ;
#4481 = DIRECTION ( 'NONE',  ( -0.7343588774761952154, 0.6787614006938686995, 0.000000000000000000 ) ) ;
#4482 = LINE ( 'NONE', #193, #18066 ) ;
#4483 = VECTOR ( 'NONE', #21947, 1000.000000000000114 ) ;
#4484 = VERTEX_POINT ( 'NONE', #21686 ) ;
#4485 = ORIENTED_EDGE ( 'NONE', *, *, #276, .T. ) ;
#4486 = CARTESIAN_POINT ( 'NONE',  ( -27.06101787524987401, 127.9652732746794044, 17.51969639969995995 ) ) ;
#4487 = AXIS2_PLACEMENT_3D ( 'NONE', #10000, #14179, #18897 ) ;
#4488 = CIRCLE ( 'NONE', #4954, 6.000000000000005329 ) ;
#4489 = LINE ( 'NONE', #23763, #25938 ) ;
#4490 = CARTESIAN_POINT ( 'NONE',  ( -175.0000000000000000, -170.0000000000001990, -69.99999999999998579 ) ) ;
#4491 = CARTESIAN_POINT ( 'NONE',  ( 158.0000000000014211, 70.52749954957745615, 45.00000000000000000 ) ) ;
#4492 = CARTESIAN_POINT ( 'NONE',  ( 158.0000000000000284, 205.9527499549551806, 45.00000000000000000 ) ) ;
#4493 = CARTESIAN_POINT ( 'NONE',  ( -196.7918453702777128, 80.49308115506423178, 248.5795775865965993 ) ) ;
#4494 = FACE_OUTER_BOUND ( 'NONE', #13436, .T. ) ;
#4495 = ORIENTED_EDGE ( 'NONE', *, *, #8739, .T. ) ;
#4496 =( REPRESENTATION_RELATIONSHIP ('NONE','NONE', #11963, #26803 ) REPRESENTATION_RELATIONSHIP_WITH_TRANSFORMATION ( #14959 )SHAPE_REPRESENTATION_RELATIONSHIP( ) );
#4497 = CARTESIAN_POINT ( 'NONE',  ( -205.1370039499190625, 144.1304017549904586, -13.00000000000000000 ) ) ;
#4498 = EDGE_CURVE ( 'NONE', #14755, #19061, #10914, .T. ) ;
#4499 = CARTESIAN_POINT ( 'NONE',  ( 217.4999999999996305, 83.06687458711267880, 36.86484227207694175 ) ) ;
#4500 = DIRECTION ( 'NONE',  ( 0.8916010070297345491, 0.4528218681375306698, 0.000000000000000000 ) ) ;
#4501 = LINE ( 'NONE', #8972, #25399 ) ;
#4502 = ORIENTED_EDGE ( 'NONE', *, *, #9093, .T. ) ;
#4503 = ADVANCED_FACE ( 'NONE', ( #28133 ), #8757, .F. ) ;
#4504 = CARTESIAN_POINT ( 'NONE',  ( -211.3876077005476759, 59.97725620786452083, 16.20275295307625996 ) ) ;
#4505 = EDGE_CURVE ( 'NONE', #4212, #27414, #17508, .T. ) ;
#4506 = ORIENTED_EDGE ( 'NONE', *, *, #27962, .F. ) ;
#4507 = VECTOR ( 'NONE', #8333, 1000.000000000000000 ) ;
#4508 = EDGE_CURVE ( 'NONE', #19398, #22237, #2277, .T. ) ;
#4509 = CARTESIAN_POINT ( 'NONE',  ( 79.99999999999994316, -70.00000000000002842, 70.00000000000001421 ) ) ;
#4510 = DIRECTION ( 'NONE',  ( 0.000000000000000000, 0.000000000000000000, 1.000000000000000000 ) ) ;
#4511 = CARTESIAN_POINT ( 'NONE',  ( -50.01279441628821587, 86.62470095750859400, 45.00000000000000000 ) ) ;
#4512 = ORIENTED_EDGE ( 'NONE', *, *, #23837, .F. ) ;
#4513 = LINE ( 'NONE', #19612, #6035 ) ;
#4514 = FILL_AREA_STYLE_COLOUR ( '', #15716 ) ;
#4515 = ORIENTED_EDGE ( 'NONE', *, *, #17446, .F. ) ;
#4516 = AXIS2_PLACEMENT_3D ( 'NONE', #1651, #10709, #21333 ) ;
#4517 = DIRECTION ( 'NONE',  ( -0.000000000000000000, -0.000000000000000000, -1.000000000000000000 ) ) ;
#4518 = ORIENTED_EDGE ( 'NONE', *, *, #9974, .T. ) ;
#4519 = CARTESIAN_POINT ( 'NONE',  ( -268.1249842685929821, -165.6674762674429076, 109.3623863443581570 ) ) ;
#4520 = VECTOR ( 'NONE', #5991, 1000.000000000000000 ) ;
#4521 = ORIENTED_EDGE ( 'NONE', *, *, #14366, .T. ) ;
#4522 = ORIENTED_EDGE ( 'NONE', *, *, #13546, .T. ) ;
#4523 = LINE ( 'NONE', #13310, #21391 ) ;
#4524 = ORIENTED_EDGE ( 'NONE', *, *, #10490, .T. ) ;
#4525 = VERTEX_POINT ( 'NONE', #15086 ) ;
#4526 = FACE_OUTER_BOUND ( 'NONE', #7222, .T. ) ;
#4527 = CARTESIAN_POINT ( 'NONE',  ( 88.44954299047319068, 230.0000000005625225, 16.19779584935177041 ) ) ;
#4528 = AXIS2_PLACEMENT_3D ( 'NONE', #22625, #921, #27062 ) ;
#4529 = DIRECTION ( 'NONE',  ( 0.000000000000000000, 1.214306433183764966E-16, -1.000000000000000000 ) ) ;
#4530 = CARTESIAN_POINT ( 'NONE',  ( 157.4999999999996589, 273.9193126614005678, 45.00000000000000000 ) ) ;
#4531 = EDGE_CURVE ( 'NONE', #21598, #583, #8617, .T. ) ;
#4532 = LINE ( 'NONE', #24093, #4572 ) ;
#4533 = AXIS2_PLACEMENT_3D ( 'NONE', #20666, #18523, #20098 ) ;
#4534 = ADVANCED_FACE ( 'NONE', ( #11056 ), #19809, .F. ) ;
#4535 = CARTESIAN_POINT ( 'NONE',  ( 65.00000000000000000, -170.0000000000000568, 70.00000000000001421 ) ) ;
#4536 = DIRECTION ( 'NONE',  ( 1.000000000000000000, 0.000000000000000000, -0.000000000000000000 ) ) ;
#4537 = PRODUCT ( 'Handel High-Force Electromagnet Base Block', 'Handel High-Force Electromagnet Base Block', '', ( #21552 ) ) ;
#4538 = CARTESIAN_POINT ( 'NONE',  ( 157.9999999999997442, 256.1102501050980322, 45.00000000000000000 ) ) ;
#4539 = CARTESIAN_POINT ( 'NONE',  ( 179.9999999999999147, 330.0000000000000000, -100.0000000000000142 ) ) ;
#4540 = LINE ( 'NONE', #15626, #22995 ) ;
#4541 = FACE_BOUND ( 'NONE', #24827, .T. ) ;
#4542 = FACE_OUTER_BOUND ( 'NONE', #17105, .T. ) ;
#4543 = ORIENTED_EDGE ( 'NONE', *, *, #1867, .T. ) ;
#4544 = FACE_OUTER_BOUND ( 'NONE', #11580, .T. ) ;
#4545 = VECTOR ( 'NONE', #1147, 1000.000000000000000 ) ;
#4546 = ADVANCED_FACE ( 'NONE', ( #13650 ), #25572, .T. ) ;
#4547 = ADVANCED_FACE ( 'NONE', ( #16234 ), #13694, .T. ) ;
#4548 = CARTESIAN_POINT ( 'NONE',  ( 157.9999999999997442, 251.6023750975910218, 45.00000000000000000 ) ) ;
#4549 = FACE_OUTER_BOUND ( 'NONE', #12039, .T. ) ;
#4550 = CARTESIAN_POINT ( 'NONE',  ( 108.2714812867982488, 206.3715290211474382, -139.1934629298939683 ) ) ;
#4551 = ORIENTED_EDGE ( 'NONE', *, *, #18218, .F. ) ;
#4552 = VECTOR ( 'NONE', #15618, 1000.000000000000000 ) ;
#4553 = DIRECTION ( 'NONE',  ( 0.8916010070290389944, -0.4528218681389001854, 0.000000000000000000 ) ) ;
#4554 = VERTEX_POINT ( 'NONE', #20238 ) ;
#4555 = CARTESIAN_POINT ( 'NONE',  ( 367.9108539694884144, 44.41075299063183479, 167.7200181511720416 ) ) ;
#4556 = ORIENTED_EDGE ( 'NONE', *, *, #4352, .T. ) ;
#4557 = AXIS2_PLACEMENT_3D ( 'NONE', #482, #628, #13708 ) ;
#4558 = ORIENTED_EDGE ( 'NONE', *, *, #1454, .F. ) ;
#4559 = AXIS2_PLACEMENT_3D ( 'NONE', #24106, #4409, #11031 ) ;
#4560 = EDGE_LOOP ( 'NONE', ( #14387, #3504, #4108, #8676 ) ) ;
#4561 = ORIENTED_EDGE ( 'NONE', *, *, #16547, .F. ) ;
#4562 = VERTEX_POINT ( 'NONE', #22830 ) ;
#4563 = CARTESIAN_POINT ( 'NONE',  ( 232.4749999999995964, 133.0668745871126930, 30.86484227207697018 ) ) ;
#4564 = VECTOR ( 'NONE', #13075, 1000.000000000000000 ) ;
#4565 = DIRECTION ( 'NONE',  ( 0.000000000000000000, 0.000000000000000000, 1.000000000000000000 ) ) ;
#4566 = UNCERTAINTY_MEASURE_WITH_UNIT (LENGTH_MEASURE( 1.000000000000000082E-05 ), #22156, 'distance_accuracy_value', 'NONE');
#4567 = CARTESIAN_POINT ( 'NONE',  ( 232.4999999999996305, 83.06687458711267880, 36.86484227207694175 ) ) ;
#4568 = CARTESIAN_POINT ( 'NONE',  ( -226.8880901706932605, 73.06320664976882995, 17.43415524067561861 ) ) ;
#4569 = DIRECTION ( 'NONE',  ( 0.000000000000000000, -1.000000000000000000, 0.000000000000000000 ) ) ;
#4570 = EDGE_CURVE ( 'NONE', #20676, #27164, #23761, .T. ) ;
#4571 = CYLINDRICAL_SURFACE ( 'NONE', #9915, 5.000000000000000888 ) ;
#4572 = VECTOR ( 'NONE', #22360, 1000.000000000000000 ) ;
#4573 = DIRECTION ( 'NONE',  ( -0.000000000000000000, -0.000000000000000000, -1.000000000000000000 ) ) ;
#4574 = CARTESIAN_POINT ( 'NONE',  ( 112.4999999999998863, 220.0000000000000284, -105.0000000000000284 ) ) ;
#4575 = CARTESIAN_POINT ( 'NONE',  ( 135.1062353973271968, 7.258260926501912458, 45.00000000000000000 ) ) ;
#4576 = CARTESIAN_POINT ( 'NONE',  ( 107.3061218092289408, 127.3934823308085242, 87.81249999970602005 ) ) ;
#4577 = AXIS2_PLACEMENT_3D ( 'NONE', #5968, #16756, #1237 ) ;
#4578 = CARTESIAN_POINT ( 'NONE',  ( -4.279759758627867505, 134.1644510977413915, 13.92782111787041899 ) ) ;
#4579 = CARTESIAN_POINT ( 'NONE',  ( -207.9699968406354458, 74.12752936445579621, 42.75546270459319231 ) ) ;
#4580 = LINE ( 'NONE', #11205, #9247 ) ;
#4581 = LINE ( 'NONE', #11062, #27172 ) ;
#4583 = VERTEX_POINT ( 'NONE', #2710 ) ;
#4582 = ORIENTED_EDGE ( 'NONE', *, *, #16178, .F. ) ;
#4584 = CARTESIAN_POINT ( 'NONE',  ( -173.3845272153682515, 113.8923293831577013, 27.65784535673404676 ) ) ;
#4585 = EDGE_CURVE ( 'NONE', #15391, #14406, #20095, .T. ) ;
#4586 = B_SPLINE_CURVE_WITH_KNOTS ( 'NONE', 3,
 ( #27798, #5974, #8564, #23504, #3818, #12604, #25516, #26073, #23360, #24497, #26215, #8839, #20184, #8701, #6542, #21913, #4805, #18035, #26638, #26355, #15324, #6820, #13591, #11438, #22343, #15465, #7115, #225, #17599, #17889, #2651, #13443, #15604, #2217, #11142, #512, #24076, #4379 ),
 .UNSPECIFIED., .F., .F.,
 ( 4, 2, 2, 2, 2, 2, 2, 2, 2, 2, 2, 2, 2, 2, 2, 2, 2, 2, 4 ),
 ( 0.000000000000000000, 0.003119048492555984414, 0.006238096985111968827, 0.007797621231389974261, 0.009357145477667980563, 0.01247619397022393418, 0.01403571821650191620, 0.01559524246277989822, 0.01871429095533593337, 0.02027381520161395528, 0.02183333944789197373, 0.02495238794044801409, 0.03119048492556014684, 0.03742858191067228307, 0.04054763040322835466, 0.04210715464950640086, 0.04366667889578444706, 0.04678572738834055333, 0.04990477588089665961 ),
 .UNSPECIFIED. ) ;
#4587 = LINE ( 'NONE', #13232, #16771 ) ;
#4588 = EDGE_LOOP ( 'NONE', ( #10333, #654 ) ) ;
#4589 = ORIENTED_EDGE ( 'NONE', *, *, #3228, .F. ) ;
#4590 = ORIENTED_EDGE ( 'NONE', *, *, #22306, .T. ) ;
#4591 = DIRECTION ( 'NONE',  ( 0.4528218681382319422, -0.8916010070293783896, 0.000000000000000000 ) ) ;
#4592 = CARTESIAN_POINT ( 'NONE',  ( -108.0188924393233947, 135.2207200644698446, 13.71980004753943483 ) ) ;
#4593 = ORIENTED_EDGE ( 'NONE', *, *, #25750, .T. ) ;
#4594 = ADVANCED_FACE ( 'NONE', ( #11646 ), #26496, .T. ) ;
#4595 = LINE ( 'NONE', #13380, #13183 ) ;
#4596 = CIRCLE ( 'NONE', #11500, 19.99999999999998934 ) ;
#4597 = EDGE_CURVE ( 'NONE', #16382, #8245, #20384, .T. ) ;
#4598 = DIRECTION ( 'NONE',  ( -0.000000000000000000, -0.000000000000000000, -1.000000000000000000 ) ) ;
#4599 = EDGE_LOOP ( 'NONE', ( #4952, #27489, #9694, #21317 ) ) ;
#4600 = CARTESIAN_POINT ( 'NONE',  ( -208.5124701773697211, 89.65907251580088655, 24.74122501709897293 ) ) ;
#4601 = DIRECTION ( 'NONE',  ( 8.673617379884074915E-17, 1.000000000000000000, -0.000000000000000000 ) ) ;
#4602 = EDGE_CURVE ( 'NONE', #12113, #22238, #26549, .T. ) ;
#4603 = CARTESIAN_POINT ( 'NONE',  ( 39.99999999999996447, 59.99999999999981526, 100.0000000000000142 ) ) ;
#4604 = CARTESIAN_POINT ( 'NONE',  ( 160.7820054808089196, 204.6557434137805274, -151.0000000000000568 ) ) ;
#4605 = ORIENTED_EDGE ( 'NONE', *, *, #12094, .F. ) ;
#4606 = CARTESIAN_POINT ( 'NONE',  ( 157.4999999999998579, 63.25781203080982351, -45.00000000000000000 ) ) ;
#4607 = DIRECTION ( 'NONE',  ( 0.000000000000000000, 0.000000000000000000, -1.000000000000000000 ) ) ;
#4608 = CARTESIAN_POINT ( 'NONE',  ( -210.0000000000000568, -220.0000000000000853, -89.99999999999987210 ) ) ;
#4609 = CARTESIAN_POINT ( 'NONE',  ( 158.0000000000000853, 196.4291249324366504, 45.00000000000000000 ) ) ;
#4610 = ORIENTED_EDGE ( 'NONE', *, *, #14135, .T. ) ;
#4611 = CARTESIAN_POINT ( 'NONE',  ( -211.0655007229363207, -220.0000000000000568, -108.1818347287491378 ) ) ;
#4612 = ADVANCED_FACE ( 'NONE', ( #7028 ), #26850, .F. ) ;
#4613 = VECTOR ( 'NONE', #12978, 1000.000000000000114 ) ;
#4614 = ADVANCED_FACE ( 'NONE', ( #11787 ), #17789, .T. ) ;
#4615 = DIRECTION ( 'NONE',  ( 1.000000000000000000, 1.850371707708593823E-16, 0.000000000000000000 ) ) ;
#4616 = CARTESIAN_POINT ( 'NONE',  ( 157.4999999999998579, 141.0019372635281627, -45.00000000000000000 ) ) ;
#4617 = VERTEX_POINT ( 'NONE', #24698 ) ;
#4618 =( NAMED_UNIT ( * ) PLANE_ANGLE_UNIT ( ) SI_UNIT ( $, .RADIAN. ) );
#4619 = VERTEX_POINT ( 'NONE', #713 ) ;
#4620 = LINE ( 'NONE', #19860, #10635 ) ;
#4621 = CARTESIAN_POINT ( 'NONE',  ( 157.4999999999998579, 151.0334372935563465, 45.00000000000000000 ) ) ;
#4622 = EDGE_LOOP ( 'NONE', ( #20541, #11941, #19367, #21894 ) ) ;
#4624 = EDGE_CURVE ( 'NONE', #9708, #968, #5408, .T. ) ;
#4623 = VERTEX_POINT ( 'NONE', #9482 ) ;
#4625 = DIRECTION ( 'NONE',  ( -0.8916010070293383105, -0.4528218681383106015, 0.000000000000000000 ) ) ;
#4626 = CARTESIAN_POINT ( 'NONE',  ( 0.000000000000000000, 0.000000000000000000, 0.000000000000000000 ) ) ;
#4627 = ORIENTED_EDGE ( 'NONE', *, *, #12476, .F. ) ;
#4628 = ORIENTED_EDGE ( 'NONE', *, *, #21147, .F. ) ;
#4629 = EDGE_CURVE ( 'NONE', #1528, #3222, #19165, .T. ) ;
#4630 = PLANE ( 'NONE',  #13448 ) ;
#4631 = EDGE_CURVE ( 'NONE', #27697, #7917, #24407, .T. ) ;
#4632 = VECTOR ( 'NONE', #2570, 1000.000000000000000 ) ;
#4633 = DIRECTION ( 'NONE',  ( 1.000000000000000000, 0.000000000000000000, 0.000000000000000000 ) ) ;
#4634 = ADVANCED_FACE ( 'NONE', ( #20525 ), #7462, .F. ) ;
#4635 = DIRECTION ( 'NONE',  ( -0.000000000000000000, -0.000000000000000000, -1.000000000000000000 ) ) ;
#4636 = DIRECTION ( 'NONE',  ( 0.000000000000000000, 0.2756732917354685064, -0.9612513907525602752 ) ) ;
#4637 = LINE ( 'NONE', #27952, #13713 ) ;
#4638 = CARTESIAN_POINT ( 'NONE',  ( -208.4180627997079114, 72.50595385281455663, -40.62079366388483237 ) ) ;
#4639 = CARTESIAN_POINT ( 'NONE',  ( 187.4999999999996305, 83.06687458711267880, 42.86484227207692754 ) ) ;
#4640 = ORIENTED_EDGE ( 'NONE', *, *, #3119, .T. ) ;
#4641 = DIRECTION ( 'NONE',  ( 0.000000000000000000, 1.214306433183764966E-16, -1.000000000000000000 ) ) ;
#4642 = CARTESIAN_POINT ( 'NONE',  ( 109.9999999999999289, -40.00000000000002842, 100.0000000000000142 ) ) ;
#4643 = LINE ( 'NONE', #24484, #11893 ) ;
#4644 = CARTESIAN_POINT ( 'NONE',  ( 158.0000000000005684, 151.2873747973098659, 45.00000000000000000 ) ) ;
#4645 = ORIENTED_EDGE ( 'NONE', *, *, #18540, .F. ) ;
#4646 = DIRECTION ( 'NONE',  ( -0.000000000000000000, 0.000000000000000000, 1.000000000000000000 ) ) ;
#4647 = VERTEX_POINT ( 'NONE', #24981 ) ;
#4648 = VECTOR ( 'NONE', #27787, 999.9999999999998863 ) ;
#4649 = DIRECTION ( 'NONE',  ( -0.000000000000000000, -1.000000000000000000, -0.000000000000000000 ) ) ;
#4650 = CARTESIAN_POINT ( 'NONE',  ( -217.3069758534620632, 60.48634897156497203, -12.43751791598376499 ) ) ;
#4651 = CARTESIAN_POINT ( 'NONE',  ( 140.1965873975519230, 249.5466472113101872, -141.9943226514402568 ) ) ;
#4652 = ORIENTED_EDGE ( 'NONE', *, *, #15149, .T. ) ;
#4653 = SURFACE_STYLE_USAGE ( .BOTH. , #3952 ) ;
#4654 = CARTESIAN_POINT ( 'NONE',  ( -295.0000000000001705, -152.0000000000000284, 60.00000000000002842 ) ) ;
#4655 = EDGE_CURVE ( 'NONE', #21098, #10156, #2564, .T. ) ;
#4656 = VECTOR ( 'NONE', #1629, 1000.000000000000000 ) ;
#4657 = VERTEX_POINT ( 'NONE', #24553 ) ;
#4658 = CIRCLE ( 'NONE', #6486, 35.00000000000002842 ) ;
#4659 = AXIS2_PLACEMENT_3D ( 'NONE', #8875, #4689, #13476 ) ;
#4660 = CARTESIAN_POINT ( 'NONE',  ( 217.4749999999996533, 258.6181251126050711, 1.387778780781445676E-14 ) ) ;
#4661 = VERTEX_POINT ( 'NONE', #14494 ) ;
#4662 = CARTESIAN_POINT ( 'NONE',  ( -274.7321073701114642, -170.0332518446063830, 91.86918944433702450 ) ) ;
#4663 = ORIENTED_EDGE ( 'NONE', *, *, #15827, .F. ) ;
#4664 = ORIENTED_EDGE ( 'NONE', *, *, #8488, .T. ) ;
#4665 = CARTESIAN_POINT ( 'NONE',  ( 158.0000000000006537, 145.7637497747887210, 45.00000000000000000 ) ) ;
#4666 = EDGE_LOOP ( 'NONE', ( #24349, #9197, #9281, #2051 ) ) ;
#4667 = VERTEX_POINT ( 'NONE', #5717 ) ;
#4668 = EDGE_LOOP ( 'NONE', ( #27210, #5943, #23758, #8744 ) ) ;
#4669 = ADVANCED_FACE ( 'NONE', ( #3415 ), #3843, .F. ) ;
#4670 = CARTESIAN_POINT ( 'NONE',  ( 92.04920872066333004, 230.5961997032264037, 17.50980340463666707 ) ) ;
#4671 = EDGE_CURVE ( 'NONE', #19265, #27055, #7739, .T. ) ;
#4672 = VECTOR ( 'NONE', #19004, 1000.000000000000000 ) ;
#4673 = DIRECTION ( 'NONE',  ( -1.000000000000000000, 3.700743415417191886E-15, 0.000000000000000000 ) ) ;
#4674 = CARTESIAN_POINT ( 'NONE',  ( 157.4999999999998579, 158.5570623160774630, 45.00000000000000000 ) ) ;
#4675 = CIRCLE ( 'NONE', #8361, 5.999999999999991118 ) ;
#4676 = VECTOR ( 'NONE', #19046, 1000.000000000000114 ) ;
#4677 = DIRECTION ( 'NONE',  ( -4.625929269271484928E-16, 1.000000000000000000, 0.000000000000000000 ) ) ;
#4678 = DIRECTION ( 'NONE',  ( -0.000000000000000000, -0.000000000000000000, 1.000000000000000000 ) ) ;
#4679 = FACE_OUTER_BOUND ( 'NONE', #23256, .T. ) ;
#4680 = CARTESIAN_POINT ( 'NONE',  ( -277.2150368962633706, -170.0000000000001137, -90.47363622314027509 ) ) ;
#4681 = DIRECTION ( 'NONE',  ( 1.000000000000000000, 0.000000000000000000, -0.000000000000000000 ) ) ;
#4682 = CARTESIAN_POINT ( 'NONE',  ( 158.0000000000015916, 53.48024950453520177, 45.00000000000000000 ) ) ;
#4683 = CARTESIAN_POINT ( 'NONE',  ( -221.3650667873343139, -91.18033988749901653, 0.000000000000000000 ) ) ;
#4684 = ORIENTED_EDGE ( 'NONE', *, *, #7416, .T. ) ;
#4685 = CARTESIAN_POINT ( 'NONE',  ( -160.0000000000000284, 118.4170923319166633, 21.37420696376539198 ) ) ;
#4686 = ADVANCED_FACE ( 'NONE', ( #12486 ), #10178, .F. ) ;
#4687 = DIRECTION ( 'NONE',  ( 0.000000000000000000, -1.000000000000000000, 0.000000000000000000 ) ) ;
#4688 = CARTESIAN_POINT ( 'NONE',  ( -68.57415822541635464, 29.64876300893806516, 95.00000000000000000 ) ) ;
#4689 = DIRECTION ( 'NONE',  ( -0.000000000000000000, 1.000000000000000000, -1.387778780781445429E-16 ) ) ;
#4690 = ORIENTED_EDGE ( 'NONE', *, *, #6020, .F. ) ;
#4691 = AXIS2_PLACEMENT_3D ( 'NONE', #9033, #15649, #22243 ) ;
#4692 = VECTOR ( 'NONE', #19679, 1000.000000000000000 ) ;
#4693 = CARTESIAN_POINT ( 'NONE',  ( 109.8801565119820935, 257.7417414023324795, -41.08725989922736233 ) ) ;
#4694 = EDGE_LOOP ( 'NONE', ( #27857, #21716, #27142, #10641, #26323 ) ) ;
#4695 = DIRECTION ( 'NONE',  ( 1.000000000000000000, 0.000000000000000000, 0.000000000000000000 ) ) ;
#4696 = ORIENTED_EDGE ( 'NONE', *, *, #371, .T. ) ;
#4697 = VECTOR ( 'NONE', #1553, 1000.000000000000000 ) ;
#4698 = ORIENTED_EDGE ( 'NONE', *, *, #10927, .T. ) ;
#4699 = CIRCLE ( 'NONE', #18477, 10.71881775658151170 ) ;
#4700 = ORIENTED_EDGE ( 'NONE', *, *, #26969, .F. ) ;
#4701 = ORIENTED_EDGE ( 'NONE', *, *, #20546, .F. ) ;
#4702 = EDGE_CURVE ( 'NONE', #5949, #12519, #23528, .T. ) ;
#4703 = ORIENTED_EDGE ( 'NONE', *, *, #3904, .T. ) ;
#4704 = LINE ( 'NONE', #2406, #13661 ) ;
#4705 = LINE ( 'NONE', #24830, #810 ) ;
#4706 = LINE ( 'NONE', #22386, #18014 ) ;
#4707 = EDGE_CURVE ( 'NONE', #15896, #23283, #21458, .T. ) ;
#4708 = ADVANCED_FACE ( 'NONE', ( #18520 ), #16434, .F. ) ;
#4709 = FACE_OUTER_BOUND ( 'NONE', #16659, .T. ) ;
#4710 = LINE ( 'NONE', #13496, #18511 ) ;
#4711 = VECTOR ( 'NONE', #10695, 1000.000000000000114 ) ;
#4712 = CARTESIAN_POINT ( 'NONE',  ( -213.4585383333369180, 57.78353604556346568, 35.98283585096940129 ) ) ;
#4713 = CARTESIAN_POINT ( 'NONE',  ( 157.4999999999998579, 98.36806213590843129, 45.00000000000000000 ) ) ;
#4714 = FACE_OUTER_BOUND ( 'NONE', #3139, .T. ) ;
#4715 = AXIS2_PLACEMENT_3D ( 'NONE', #6393, #6677, #17590 ) ;
#4716 = LINE ( 'NONE', #13500, #27780 ) ;
#4717 = FACE_OUTER_BOUND ( 'NONE', #28226, .T. ) ;
#4718 = AXIS2_PLACEMENT_3D ( 'NONE', #4683, #6991, #20493 ) ;
#4719 = CARTESIAN_POINT ( 'NONE',  ( 157.4999999999998579, 115.9231871884577174, 45.00000000000000000 ) ) ;
#4720 = CARTESIAN_POINT ( 'NONE',  ( 232.4999999999996305, 494.4107529906318632, 75.35061095560301681 ) ) ;
#4721 = AXIS2_PLACEMENT_3D ( 'NONE', #22669, #14189, #9870 ) ;
#4722 = CARTESIAN_POINT ( 'NONE',  ( 6.333667032819452203, 140.1905188151071968, 13.00000000068521011 ) ) ;
#4723 = DIRECTION ( 'NONE',  ( 0.4528218681376112720, 0.8916010070296936929, -0.000000000000000000 ) ) ;
#4724 = CARTESIAN_POINT ( 'NONE',  ( 158.0000000000009379, 118.1771246922112653, 45.00000000000000000 ) ) ;
#4725 = CARTESIAN_POINT ( 'NONE',  ( 154.8288972274760908, 217.3894761555990556, 45.00000000000000000 ) ) ;
#4726 = B_SPLINE_CURVE_WITH_KNOTS ( 'NONE', 3,
 ( #14384, #9791, #18965, #3583, #1017, #1433, #7906, #8186, #18547, #16400, #12096, #27709, #16953, #8047, #25706, #16538, #16815, #25561, #6029, #1297, #14810, #1157, #5465, #23140, #27293, #23415, #3724, #7633, #12515, #23561, #11951, #25145, #14247, #18682, #20693, #22996, #25287, #3445, #21836, #8759, #26134, #4152 ),
 .UNSPECIFIED., .F., .F.,
 ( 4, 2, 2, 2, 2, 2, 2, 2, 2, 2, 2, 2, 2, 2, 2, 2, 2, 2, 2, 2, 4 ),
 ( 0.01880622955133634880, 0.01998131524074750476, 0.02115640093015866419, 0.02174394377486424737, 0.02233148661956983055, 0.02350657230898089631, 0.02468165799839196206, 0.02585674368780302781, 0.02644428653250854855, 0.02703182937721406581, 0.02820691506662520789, 0.02938200075603634651, 0.03055708644544748859, 0.03173217213485862720, 0.03231971497956417916, 0.03290725782426972418, 0.03408234351368071013, 0.03525742920309170303, 0.03584497204779715784, 0.03643251489250261960, 0.03760760058191347371 ),
 .UNSPECIFIED. ) ;
#4728 = ORIENTED_EDGE ( 'NONE', *, *, #1442, .T. ) ;
#4727 = ORIENTED_EDGE ( 'NONE', *, *, #19536, .F. ) ;
#4729 = CARTESIAN_POINT ( 'NONE',  ( 125.3433571860711453, 242.0587615242396566, 84.99999999999995737 ) ) ;
#4730 = DIRECTION ( 'NONE',  ( 0.000000000000000000, 0.000000000000000000, -1.000000000000000000 ) ) ;
#4731 = CARTESIAN_POINT ( 'NONE',  ( -207.8550219111573369, 89.23948686170545841, -26.88820707009881161 ) ) ;
#4732 = ORIENTED_EDGE ( 'NONE', *, *, #1128, .T. ) ;
#4733 = ORIENTED_EDGE ( 'NONE', *, *, #22007, .T. ) ;
#4734 = VECTOR ( 'NONE', #27013, 999.9999999999998863 ) ;
#4735 = ORIENTED_EDGE ( 'NONE', *, *, #20897, .F. ) ;
#4736 = EDGE_CURVE ( 'NONE', #9830, #15470, #16371, .T. ) ;
#4737 = VECTOR ( 'NONE', #6075, 1000.000000000000000 ) ;
#4738 = DIRECTION ( 'NONE',  ( 0.000000000000000000, 0.000000000000000000, 1.000000000000000000 ) ) ;
#4739 = CARTESIAN_POINT ( 'NONE',  ( -295.0000000000001705, -165.0000000000001137, -59.99999999999986500 ) ) ;
#4740 = VERTEX_POINT ( 'NONE', #3269 ) ;
#4741 = VECTOR ( 'NONE', #24665, 1000.000000000000000 ) ;
#4742 = VERTEX_POINT ( 'NONE', #7875 ) ;
#4743 = DIRECTION ( 'NONE',  ( -0.8916010070298961976, 0.4528218681372121468, 0.000000000000000000 ) ) ;
#4744 = ADVANCED_FACE ( 'NONE', ( #14351 ), #20810, .F. ) ;
#4745 = FACE_OUTER_BOUND ( 'NONE', #22806, .T. ) ;
#4746 = ORIENTED_EDGE ( 'NONE', *, *, #27218, .F. ) ;
#4747 = DIRECTION ( 'NONE',  ( -1.000000000000000000, -1.321694076934710155E-16, 0.000000000000000000 ) ) ;
#4748 = CARTESIAN_POINT ( 'NONE',  ( 157.9999999999996589, 273.6653751576470768, -45.00000000000000000 ) ) ;
#4749 = ADVANCED_FACE ( 'NONE', ( #18934 ), #26051, .T. ) ;
#4750 = CARTESIAN_POINT ( 'NONE',  ( 157.9999999999999147, 213.9842499849850697, 45.00000000000000000 ) ) ;
#4751 = DIRECTION ( 'NONE',  ( 1.000000000000000000, 0.000000000000000000, 0.000000000000000000 ) ) ;
#4752 = CARTESIAN_POINT ( 'NONE',  ( -215.3329573321002783, 58.91837420257471081, -30.17944279518760098 ) ) ;
#4753 = AXIS2_PLACEMENT_3D ( 'NONE', #17156, #3795, #6377 ) ;
#4754 = ORIENTED_EDGE ( 'NONE', *, *, #19042, .T. ) ;
#4755 = CARTESIAN_POINT ( 'NONE',  ( 157.4999999999998579, 156.0491873085704242, 45.00000000000000000 ) ) ;
#4756 = DIRECTION ( 'NONE',  ( 1.000000000000000000, -0.000000000000000000, -0.000000000000000000 ) ) ;
#4757 = DIRECTION ( 'NONE',  ( 1.000000000000000000, 0.000000000000000000, -2.775557561562887407E-16 ) ) ;
#4758 = VECTOR ( 'NONE', #8691, 1000.000000000000114 ) ;
#4759 = LINE ( 'NONE', #8163, #18997 ) ;
#4760 = ORIENTED_EDGE ( 'NONE', *, *, #16462, .F. ) ;
#4761 = EDGE_CURVE ( 'NONE', #27481, #21665, #17341, .T. ) ;
#4762 = CARTESIAN_POINT ( 'NONE',  ( 0.000000000000000000, -18.01420295945611727, 100.0000000000000000 ) ) ;
#4763 = DIRECTION ( 'NONE',  ( 0.000000000000000000, 0.000000000000000000, -1.000000000000000000 ) ) ;
#4764 = CARTESIAN_POINT ( 'NONE',  ( 2.399999999999999911, -1.250000000000000444, 7.582700855991164168 ) ) ;
#4765 = ORIENTED_EDGE ( 'NONE', *, *, #15857, .F. ) ;
#4766 = SHAPE_REPRESENTATION_RELATIONSHIP ( 'NONE' , 'NONE' ,  #13220, #16401 ) ;
#4767 = ORIENTED_EDGE ( 'NONE', *, *, #2701, .F. ) ;
#4768 = EDGE_CURVE ( 'NONE', #22350, #1387, #14631, .T. ) ;
#4769 = CARTESIAN_POINT ( 'NONE',  ( 157.4999999999998010, 236.3011875487955251, 45.00000000000000000 ) ) ;
#4770 = PLANE ( 'NONE',  #11298 ) ;
#4771 = ORIENTED_EDGE ( 'NONE', *, *, #20496, .F. ) ;
#4772 = EDGE_LOOP ( 'NONE', ( #17952, #10584, #25831, #2581 ) ) ;
#4773 = DIRECTION ( 'NONE',  ( 0.05364526231779676024, 0.9985600561963485777, 0.000000000000000000 ) ) ;
#4774 = DIRECTION ( 'NONE',  ( 1.000000000000000000, 0.000000000000000000, 0.000000000000000000 ) ) ;
#4775 = ORIENTED_EDGE ( 'NONE', *, *, #8346, .T. ) ;
#4776 = VERTEX_POINT ( 'NONE', #18792 ) ;
#4777 = VECTOR ( 'NONE', #16926, 999.9999999999998863 ) ;
#4778 = CARTESIAN_POINT ( 'NONE',  ( 5.539884921987776600, 137.3884131596613258, 15.09220095556929664 ) ) ;
#4779 = ADVANCED_FACE ( 'NONE', ( #27819 ), #27395, .F. ) ;
#4780 = EDGE_CURVE ( 'NONE', #2799, #11964, #27681, .T. ) ;
#4781 = DIRECTION ( 'NONE',  ( 1.000000000000000000, -0.000000000000000000, -0.000000000000000000 ) ) ;
#4782 = CARTESIAN_POINT ( 'NONE',  ( 158.0000000000005684, 153.2873747973098659, 45.00000000000000000 ) ) ;
#4783 = CARTESIAN_POINT ( 'NONE',  ( 8.117852850209605009, 141.5785587194356197, -13.00000000000000000 ) ) ;
#4784 = FACE_OUTER_BOUND ( 'NONE', #15835, .T. ) ;
#4785 = CARTESIAN_POINT ( 'NONE',  ( -207.9673235353189682, 74.11717653937235184, -42.76310609277111041 ) ) ;
#4786 = CARTESIAN_POINT ( 'NONE',  ( -187.8924994060663494, 156.4650759647683742, 12.99999999999999822 ) ) ;
#4787 = EDGE_LOOP ( 'NONE', ( #10218, #10585, #21921, #10657 ) ) ;
#4788 = DIRECTION ( 'NONE',  ( 0.000000000000000000, 1.214306433183764966E-16, -1.000000000000000000 ) ) ;
#4789 = DIRECTION ( 'NONE',  ( 0.000000000000000000, -1.000000000000000000, 0.000000000000000000 ) ) ;
#4790 = DIRECTION ( 'NONE',  ( -1.850371707708594366E-15, -1.000000000000000000, 0.000000000000000000 ) ) ;
#4791 = CYLINDRICAL_SURFACE ( 'NONE', #10273, 32.49120955644046660 ) ;
#4792 = ORIENTED_EDGE ( 'NONE', *, *, #27028, .T. ) ;
#4793 = VECTOR ( 'NONE', #9366, 1000.000000000000000 ) ;
#4794 = ADVANCED_FACE ( 'NONE', ( #5998 ), #21085, .F. ) ;
#4795 = DIRECTION ( 'NONE',  ( 0.4528218681379715949, 0.8916010070295107282, -0.000000000000000000 ) ) ;
#4796 = ORIENTED_EDGE ( 'NONE', *, *, #6909, .F. ) ;
#4797 = EDGE_CURVE ( 'NONE', #21744, #18881, #25537, .T. ) ;
#4798 = PLANE ( 'NONE',  #12083 ) ;
#4799 = CARTESIAN_POINT ( 'NONE',  ( -215.0412094859542833, 60.20193349634170232, -13.76727271988285750 ) ) ;
#4800 = CARTESIAN_POINT ( 'NONE',  ( 138.6601105629808899, 249.7776935521190182, -149.7704424372629717 ) ) ;
#4801 = ORIENTED_EDGE ( 'NONE', *, *, #816, .F. ) ;
#4802 = DIRECTION ( 'NONE',  ( 0.000000000000000000, 0.000000000000000000, -1.000000000000000000 ) ) ;
#4803 = CARTESIAN_POINT ( 'NONE',  ( 222.4999999999996021, 186.4134324495536248, 35.02193266779035952 ) ) ;
#4804 = EDGE_LOOP ( 'NONE', ( #16481, #20473, #3890, #24309 ) ) ;
#4805 = CARTESIAN_POINT ( 'NONE',  ( -223.8049923706243476, 71.89136757138916778, 19.05429412414824242 ) ) ;
#4806 = ORIENTED_EDGE ( 'NONE', *, *, #3032, .F. ) ;
#4807 = DIRECTION ( 'NONE',  ( 0.8916010070295213863, 0.4528218681379503341, 0.000000000000000000 ) ) ;
#4808 = VERTEX_POINT ( 'NONE', #16920 ) ;
#4809 = ADVANCED_FACE ( 'NONE', ( #2107 ), #25962, .F. ) ;
#4810 = ORIENTED_EDGE ( 'NONE', *, *, #10551, .F. ) ;
#4811 = CARTESIAN_POINT ( 'NONE',  ( 111.9999999999968878, -1.554312234475174324E-12, -45.00000000000000000 ) ) ;
#4812 = VERTEX_POINT ( 'NONE', #13055 ) ;
#4813 = AXIS2_PLACEMENT_3D ( 'NONE', #2954, #5253, #14039 ) ;
#4814 = VERTEX_POINT ( 'NONE', #17478 ) ;
#4815 = ORIENTED_EDGE ( 'NONE', *, *, #12645, .T. ) ;
#4816 = AXIS2_PLACEMENT_3D ( 'NONE', #12746, #27800, #23506 ) ;
#4817 = CARTESIAN_POINT ( 'NONE',  ( 93.75109487930637897, 231.1752187890906214, 18.33298295918253018 ) ) ;
#4818 = CARTESIAN_POINT ( 'NONE',  ( 294.9233831825460470, 127.6681916698403398, -145.0000000000000000 ) ) ;
#4819 = VECTOR ( 'NONE', #13938, 1000.000000000000000 ) ;
#4820 = CARTESIAN_POINT ( 'NONE',  ( -227.3657730843237061, 133.9833936510271997, -14.99191580167116911 ) ) ;
#4821 = VECTOR ( 'NONE', #25063, 1000.000000000000114 ) ;
#4822 = CARTESIAN_POINT ( 'NONE',  ( -125.2895325436292069, 200.2180533211636657, 12.99999999999999822 ) ) ;
#4823 = DIRECTION ( 'NONE',  ( -1.000000000000000000, 0.000000000000000000, 0.000000000000000000 ) ) ;
#4824 = FACE_OUTER_BOUND ( 'NONE', #584, .T. ) ;
#4825 = DIRECTION ( 'NONE',  ( -0.000000000000000000, -0.000000000000000000, -1.000000000000000000 ) ) ;
#4826 = DIRECTION ( 'NONE',  ( -0.000000000000000000, -0.000000000000000000, -1.000000000000000000 ) ) ;
#4827 = PLANE ( 'NONE',  #24851 ) ;
#4828 = CARTESIAN_POINT ( 'NONE',  ( -214.3828916364065833, 175.2783111443768576, -13.00000000000000000 ) ) ;
#4829 = CARTESIAN_POINT ( 'NONE',  ( 164.9999999999998579, 220.0000000000000284, -169.9999999999999716 ) ) ;
#4830 = ORIENTED_EDGE ( 'NONE', *, *, #24113, .T. ) ;
#4831 = LINE ( 'NONE', #8727, #15638 ) ;
#4832 = FACE_OUTER_BOUND ( 'NONE', #8951, .T. ) ;
#4833 = LINE ( 'NONE', #13913, #18573 ) ;
#4834 = VECTOR ( 'NONE', #26465, 1000.000000000000000 ) ;
#4835 = CARTESIAN_POINT ( 'NONE',  ( 158.0000000000009663, 111.1613746771971876, 45.00000000000000000 ) ) ;
#4836 = VERTEX_POINT ( 'NONE', #10885 ) ;
#4837 = VECTOR ( 'NONE', #6279, 1000.000000000000000 ) ;
#4838 = EDGE_CURVE ( 'NONE', #19459, #14606, #21934, .T. ) ;
#4839 = CARTESIAN_POINT ( 'NONE',  ( 109.9999999999998863, 259.1520133598112352, -44.26562200958714755 ) ) ;
#4840 = ORIENTED_EDGE ( 'NONE', *, *, #24958, .T. ) ;
#4841 = DIRECTION ( 'NONE',  ( -1.000000000000000000, 0.000000000000000000, 0.000000000000000000 ) ) ;
#4842 = AXIS2_PLACEMENT_3D ( 'NONE', #26288, #8768, #15530 ) ;
#4843 = VERTEX_POINT ( 'NONE', #21506 ) ;
#4844 = VERTEX_POINT ( 'NONE', #8589 ) ;
#4845 = ORIENTED_EDGE ( 'NONE', *, *, #11047, .F. ) ;
#4846 = EDGE_LOOP ( 'NONE', ( #27580, #494, #13805, #25717 ) ) ;
#4847 = DIRECTION ( 'NONE',  ( 1.850371707708594316E-16, -1.000000000000000000, -0.000000000000000000 ) ) ;
#4848 = DIRECTION ( 'NONE',  ( -0.000000000000000000, -0.000000000000000000, -1.000000000000000000 ) ) ;
#4849 = DIRECTION ( 'NONE',  ( -0.000000000000000000, -0.000000000000000000, -1.000000000000000000 ) ) ;
#4850 = PLANE ( 'NONE',  #14666 ) ;
#4851 = AXIS2_PLACEMENT_3D ( 'NONE', #27456, #23443, #12932 ) ;
#4852 = UNCERTAINTY_MEASURE_WITH_UNIT (LENGTH_MEASURE( 1.000000000000000082E-05 ), #24383, 'distance_accuracy_value', 'NONE');
#4853 = AXIS2_PLACEMENT_3D ( 'NONE', #28080, #21779, #19479 ) ;
#4854 = CARTESIAN_POINT ( 'NONE',  ( 157.9999999999997442, 249.0945000900840398, 45.00000000000000000 ) ) ;
#4855 = CARTESIAN_POINT ( 'NONE',  ( -208.5306448315634213, 60.03373823553869926, 18.45924612780262208 ) ) ;
#4856 = CARTESIAN_POINT ( 'NONE',  ( 157.9999999999998863, 216.4921249924925348, 45.00000000000000000 ) ) ;
#4857 = DIRECTION ( 'NONE',  ( 0.8916010070293384215, 0.4528218681383106015, 0.000000000000000000 ) ) ;
#4858 = ADVANCED_FACE ( 'NONE', ( #6281, #19775 ), #15055, .F. ) ;
#4859 = DIRECTION ( 'NONE',  ( 0.5457381880580733924, 0.8379557447115514313, 0.000000000000000000 ) ) ;
#4860 = CARTESIAN_POINT ( 'NONE',  ( -223.7378885753377347, 88.77739991535318609, -14.68536764801921279 ) ) ;
#4861 = VECTOR ( 'NONE', #12126, 999.9999999999998863 ) ;
#4862 = B_SPLINE_CURVE_WITH_KNOTS ( 'NONE', 3,
 ( #24927, #4948, #658, #13740, #18324, #14159, #27075, #5243, #14029, #22776, #9701, #3076, #18462, #27212, #7552, #16318, #25069, #5380, #2504, #10262, #27347, #12004, #10124, #14439, #20748, #14298, #16730, #1492, #18736, #12569, #9982, #5803, #1354, #19020 ),
 .UNSPECIFIED., .F., .F.,
 ( 4, 2, 2, 2, 2, 2, 2, 2, 2, 2, 2, 2, 2, 2, 2, 2, 4 ),
 ( 0.000000000000000000, 0.003147291746946911419, 0.006294583493893822837, 0.007868229367367264235, 0.009441875240840705633, 0.01258916698778760924, 0.01573645873473451112, 0.01888375048168141473, 0.02517833397557515604, 0.02832562572252201108, 0.03147291746946885571, 0.03776750096336255885, 0.04406208445725624118, 0.04720937620420308234, 0.04878302207767650639, 0.04956984501441326352, 0.05035666795115002065 ),
 .UNSPECIFIED. ) ;
#4863 = LINE ( 'NONE', #6341, #22982 ) ;
#4864 = FACE_OUTER_BOUND ( 'NONE', #12888, .T. ) ;
#4865 = CARTESIAN_POINT ( 'NONE',  ( -143.6428522700808230, 20.24192588826928585, 83.00000000000001421 ) ) ;
#4866 = DIRECTION ( 'NONE',  ( 1.000000000000000000, -0.000000000000000000, -0.000000000000000000 ) ) ;
#4867 = DIRECTION ( 'NONE',  ( 0.000000000000000000, -1.000000000000000000, 0.000000000000000000 ) ) ;
#4868 = ADVANCED_FACE ( 'NONE', ( #19355 ), #1965, .F. ) ;
#4869 = DIRECTION ( 'NONE',  ( 1.000000000000000000, -0.000000000000000000, -0.000000000000000000 ) ) ;
#4871 = ORIENTED_EDGE ( 'NONE', *, *, #15555, .F. ) ;
#4870 = ORIENTED_EDGE ( 'NONE', *, *, #7098, .F. ) ;
#4872 = LINE ( 'NONE', #7329, #1805 ) ;
#4873 = EDGE_CURVE ( 'NONE', #23798, #14035, #102, .T. ) ;
#4874 = EDGE_CURVE ( 'NONE', #25738, #8109, #28102, .T. ) ;
#4875 = CARTESIAN_POINT ( 'NONE',  ( 157.4999999999998579, 163.5728123310915407, 45.00000000000000000 ) ) ;
#4876 = EDGE_CURVE ( 'NONE', #24936, #223, #17337, .T. ) ;
#4877 = ORIENTED_EDGE ( 'NONE', *, *, #6822, .F. ) ;
#4878 = CONTEXT_DEPENDENT_SHAPE_REPRESENTATION ( #12959, #12805 ) ;
#4879 = ORIENTED_EDGE ( 'NONE', *, *, #10062, .F. ) ;
#4880 = VECTOR ( 'NONE', #6475, 1000.000000000000114 ) ;
#4881 = VERTEX_POINT ( 'NONE', #26096 ) ;
#4882 = DIRECTION ( 'NONE',  ( 0.5457381880580733924, 0.8379557447115515423, -0.000000000000000000 ) ) ;
#4883 = CARTESIAN_POINT ( 'NONE',  ( -112.7208498180836358, 133.0274648423633437, 15.80898321009636298 ) ) ;
#4884 = VERTEX_POINT ( 'NONE', #6569 ) ;
#4885 = VERTEX_POINT ( 'NONE', #8864 ) ;
#4886 = CARTESIAN_POINT ( 'NONE',  ( 151.9705627484771355, 204.4436508138959141, 45.00000000000000000 ) ) ;
#4887 = DIRECTION ( 'NONE',  ( 0.8916010070298151513, -0.4528218681373720744, 0.000000000000000000 ) ) ;
#4888 = ORIENTED_EDGE ( 'NONE', *, *, #2763, .F. ) ;
#4889 = DIRECTION ( 'NONE',  ( -0.7071067811865474617, 0.7071067811865474617, 0.000000000000000000 ) ) ;
#4890 = DIRECTION ( 'NONE',  ( 0.8916010070293584056, -0.4528218681382712996, 0.000000000000000000 ) ) ;
#4891 = PLANE ( 'NONE',  #21767 ) ;
#4892 = DIRECTION ( 'NONE',  ( -0.000000000000000000, -0.000000000000000000, 1.000000000000000000 ) ) ;
#4893 = AXIS2_PLACEMENT_3D ( 'NONE', #7966, #21031, #23615 ) ;
#4894 = CARTESIAN_POINT ( 'NONE',  ( -213.7829002709373754, 55.69945581370277665, -42.78690303009008034 ) ) ;
#4895 = EDGE_CURVE ( 'NONE', #6513, #905, #17627, .T. ) ;
#4896 = ADVANCED_FACE ( 'NONE', ( #6425 ), #10029, .T. ) ;
#4897 = ORIENTED_EDGE ( 'NONE', *, *, #8905, .T. ) ;
#4898 = DIRECTION ( 'NONE',  ( -0.000000000000000000, -0.000000000000000000, -1.000000000000000000 ) ) ;
#4899 = CARTESIAN_POINT ( 'NONE',  ( -216.6483861793058452, 139.2130420792684902, -15.04814241299435018 ) ) ;
#4900 = CARTESIAN_POINT ( 'NONE',  ( 134.9999999999998579, 220.0000000000000284, 100.0000000000000142 ) ) ;
#4901 = DIRECTION ( 'NONE',  ( -0.8916010070293584056, -0.4528218681382712996, 0.000000000000000000 ) ) ;
#4902 = VERTEX_POINT ( 'NONE', #23958 ) ;
#4903 = LINE ( 'NONE', #26893, #12393 ) ;
#4904 = ADVANCED_FACE ( 'NONE', ( #24232, #15346, #4541, #13329, #1687, #17202 ), #10455, .T. ) ;
#4905 = CARTESIAN_POINT ( 'NONE',  ( -243.4193540313498545, 74.61988491602063789, 4.999999999761307379 ) ) ;
#4906 = CARTESIAN_POINT ( 'NONE',  ( -175.0000000000000000, -170.0000000000001705, 70.00000000000001421 ) ) ;
#4907 = ORIENTED_EDGE ( 'NONE', *, *, #3753, .F. ) ;
#4908 = EDGE_LOOP ( 'NONE', ( #16731, #13620, #20336, #8023 ) ) ;
#4909 = CARTESIAN_POINT ( 'NONE',  ( 88.58553289623721128, 111.2425746091579413, 71.46484375014649970 ) ) ;
#4910 = FACE_OUTER_BOUND ( 'NONE', #12193, .T. ) ;
#4911 = ORIENTED_EDGE ( 'NONE', *, *, #9709, .T. ) ;
#4912 = AXIS2_PLACEMENT_3D ( 'NONE', #17822, #20117, #4743 ) ;
#4913 = ORIENTED_EDGE ( 'NONE', *, *, #24214, .T. ) ;
#4914 = CYLINDRICAL_SURFACE ( 'NONE', #12713, 5.000000000000004441 ) ;
#4915 = FACE_BOUND ( 'NONE', #23866, .T. ) ;
#4916 = ORIENTED_EDGE ( 'NONE', *, *, #17562, .F. ) ;
#4917 = CARTESIAN_POINT ( 'NONE',  ( 157.9999999999998579, 223.5078750075070104, 45.00000000000000000 ) ) ;
#4918 = B_SPLINE_CURVE_WITH_KNOTS ( 'NONE', 3,
 ( #25502, #10561, #5818, #10420, #10281, #8407, #21188 ),
 .UNSPECIFIED., .F., .F.,
 ( 4, 3, 4 ),
 ( 0.01306422253233231051, 0.01395283648363494430, 0.01510707358649056309 ),
 .UNSPECIFIED. ) ;
#4919 = ORIENTED_EDGE ( 'NONE', *, *, #9300, .T. ) ;
#4920 = CARTESIAN_POINT ( 'NONE',  ( 9.345921402568853509, 139.9999999999999716, -13.00000000000000000 ) ) ;
#4921 = CARTESIAN_POINT ( 'NONE',  ( 157.9999999999997442, 256.1102501050980322, 45.00000000000000000 ) ) ;
#4922 = LINE ( 'NONE', #11267, #5239 ) ;
#4923 = CARTESIAN_POINT ( 'NONE',  ( -4.329335832958885355, 134.1424492706239846, -13.93339712843492606 ) ) ;
#4924 = DIRECTION ( 'NONE',  ( -0.000000000000000000, 0.000000000000000000, -1.000000000000000000 ) ) ;
#4925 = DIRECTION ( 'NONE',  ( 0.000000000000000000, -1.000000000000000000, 0.000000000000000000 ) ) ;
#4926 = AXIS2_PLACEMENT_3D ( 'NONE', #3480, #21146, #3614 ) ;
#4927 = ADVANCED_FACE ( 'NONE', ( #12765 ), #9569, .T. ) ;
#4928 = ORIENTED_EDGE ( 'NONE', *, *, #26599, .F. ) ;
#4929 = DIRECTION ( 'NONE',  ( -0.000000000000000000, -0.000000000000000000, -1.000000000000000000 ) ) ;
#4930 = CARTESIAN_POINT ( 'NONE',  ( -63.57415822541634043, -18.01420295945611727, 100.0000000000000000 ) ) ;
#4931 = DIRECTION ( 'NONE',  ( -0.9659258262890740854, -0.2588190451024993122, 0.000000000000000000 ) ) ;
#4932 = DIRECTION ( 'NONE',  ( 0.000000000000000000, 0.000000000000000000, -1.000000000000000000 ) ) ;
#4933 = AXIS2_PLACEMENT_3D ( 'NONE', #17932, #699, #13348 ) ;
#4934 = ORIENTED_EDGE ( 'NONE', *, *, #23793, .F. ) ;
#4935 = LINE ( 'NONE', #23037, #3628 ) ;
#4936 = ORIENTED_EDGE ( 'NONE', *, *, #10894, .F. ) ;
#4937 = CARTESIAN_POINT ( 'NONE',  ( -51.90955279280624524, 193.7290884209386661, 45.00000000000000000 ) ) ;
#4938 = PLANE ( 'NONE',  #10539 ) ;
#4939 = CARTESIAN_POINT ( 'NONE',  ( 140.2062392899099734, 249.5456347581138914, -148.0084258618598767 ) ) ;
#4940 = EDGE_LOOP ( 'NONE', ( #13871, #12734, #13301, #11446 ) ) ;
#4941 = DIRECTION ( 'NONE',  ( 1.000000000000000000, 0.000000000000000000, -0.000000000000000000 ) ) ;
#4942 =( NAMED_UNIT ( * ) SI_UNIT ( $, .STERADIAN. ) SOLID_ANGLE_UNIT ( ) );
#4943 = ORIENTED_EDGE ( 'NONE', *, *, #2856, .T. ) ;
#4944 = EDGE_CURVE ( 'NONE', #25070, #5248, #7289, .T. ) ;
#4945 = FACE_OUTER_BOUND ( 'NONE', #18526, .T. ) ;
#4946 = VERTEX_POINT ( 'NONE', #14919 ) ;
#4947 = ADVANCED_FACE ( 'NONE', ( #8448 ), #25594, .F. ) ;
#4948 = CARTESIAN_POINT ( 'NONE',  ( 90.99996944231388341, 240.0000000000000568, 6.657453037605657542 ) ) ;
#4949 = ORIENTED_EDGE ( 'NONE', *, *, #7416, .F. ) ;
#4950 = EDGE_LOOP ( 'NONE', ( #2805, #16799 ) ) ;
#4951 = CARTESIAN_POINT ( 'NONE',  ( 158.0000000000011084, 100.6219996396619791, 45.00000000000000000 ) ) ;
#4952 = ORIENTED_EDGE ( 'NONE', *, *, #7787, .F. ) ;
#4953 = AXIS2_PLACEMENT_3D ( 'NONE', #3553, #18653, #10036 ) ;
#4954 = AXIS2_PLACEMENT_3D ( 'NONE', #17726, #13017, #62 ) ;
#4955 = ORIENTED_EDGE ( 'NONE', *, *, #16813, .F. ) ;
#4956 = ORIENTED_EDGE ( 'NONE', *, *, #9850, .F. ) ;
#4957 = EDGE_CURVE ( 'NONE', #3222, #23714, #14164, .T. ) ;
#4958 = CARTESIAN_POINT ( 'NONE',  ( 90.45806322831077750, 239.6644751351248317, 16.82109631826968865 ) ) ;
#4959 = EDGE_CURVE ( 'NONE', #5337, #26387, #6845, .T. ) ;
#4960 = CARTESIAN_POINT ( 'NONE',  ( -219.9082363642617111, 137.1815813412194700, 12.98324324876687186 ) ) ;
#4961 = CARTESIAN_POINT ( 'NONE',  ( 65.00000000000000000, -120.0000000000000711, 70.00000000000001421 ) ) ;
#4962 = CARTESIAN_POINT ( 'NONE',  ( 158.0000000000000853, 198.9369999399436892, 45.00000000000000000 ) ) ;
#4963 = CARTESIAN_POINT ( 'NONE',  ( 175.6862808370088089, 157.7720269260891826, 45.00000000000000000 ) ) ;
#4964 = DIRECTION ( 'NONE',  ( 1.000000000000000000, 0.000000000000000000, -2.220446049250266932E-15 ) ) ;
#4965 = PRESENTATION_LAYER_ASSIGNMENT (  '', '', ( #17353 ) ) ;
#4966 = LINE ( 'NONE', #5539, #7647 ) ;
#4967 = FACE_OUTER_BOUND ( 'NONE', #22589, .T. ) ;
#4968 = DIRECTION ( 'NONE',  ( 0.8916010070293710621, -0.4528218681382463195, 0.000000000000000000 ) ) ;
#4969 = DIRECTION ( 'NONE',  ( 0.000000000000000000, 0.000000000000000000, -1.000000000000000000 ) ) ;
#4970 = CARTESIAN_POINT ( 'NONE',  ( 157.9999999999998295, 226.5236250225210313, -45.00000000000000000 ) ) ;
#4971 = ORIENTED_EDGE ( 'NONE', *, *, #8571, .T. ) ;
#4972 = DIRECTION ( 'NONE',  ( 0.8916010070293584056, -0.4528218681382712996, 0.000000000000000000 ) ) ;
#4973 = CIRCLE ( 'NONE', #19186, 5.999999999999991118 ) ;
#4974 = VECTOR ( 'NONE', #20378, 1000.000000000000114 ) ;
#4975 = CARTESIAN_POINT ( 'NONE',  ( 79.99999999999994316, -100.0000000000000284, 100.0000000000000142 ) ) ;
#4976 = FACE_OUTER_BOUND ( 'NONE', #15902, .T. ) ;
#4977 = CARTESIAN_POINT ( 'NONE',  ( -221.3650667873343139, -91.18033988749901653, -14.94182580522077330 ) ) ;
#4978 = ORIENTED_EDGE ( 'NONE', *, *, #16413, .T. ) ;
#4979 = EDGE_CURVE ( 'NONE', #13140, #15105, #22512, .T. ) ;
#4980 = EDGE_CURVE ( 'NONE', #22380, #7575, #6342, .T. ) ;
#4981 = CARTESIAN_POINT ( 'NONE',  ( 217.4999999999996305, 194.4107529906318064, 100.0000000000000284 ) ) ;
#4982 = VERTEX_POINT ( 'NONE', #22221 ) ;
#4983 = SURFACE_STYLE_USAGE ( .BOTH. , #9872 ) ;
#4984 = ORIENTED_EDGE ( 'NONE', *, *, #5174, .T. ) ;
#4985 = AXIS2_PLACEMENT_3D ( 'NONE', #21400, #139, #10630 ) ;
#4986 = ORIENTED_EDGE ( 'NONE', *, *, #5214, .T. ) ;
#4987 = ORIENTED_EDGE ( 'NONE', *, *, #7431, .T. ) ;
#4988 = EDGE_LOOP ( 'NONE', ( #26715, #14255, #27110, #24104 ) ) ;
#4989 = CYLINDRICAL_SURFACE ( 'NONE', #7230, 53.86582179324592090 ) ;
#4990 = DIRECTION ( 'NONE',  ( 0.000000000000000000, 0.000000000000000000, -1.000000000000000000 ) ) ;
#4991 = FACE_OUTER_BOUND ( 'NONE', #4035, .T. ) ;
#4992 = CIRCLE ( 'NONE', #28371, 16.07743405327025243 ) ;
#4993 = CIRCLE ( 'NONE', #26965, 1.000000000000000888 ) ;
#4994 = CARTESIAN_POINT ( 'NONE',  ( -43.02437977270767533, 129.7200458115292747, -16.81627168235289105 ) ) ;
#4995 = EDGE_CURVE ( 'NONE', #26118, #11930, #16200, .T. ) ;
#4996 = DIRECTION ( 'NONE',  ( -0.000000000000000000, -0.000000000000000000, -1.000000000000000000 ) ) ;
#4998 = EDGE_CURVE ( 'NONE', #26005, #10330, #6990, .T. ) ;
#4997 = VECTOR ( 'NONE', #28015, 1000.000000000000000 ) ;
#4999 = CARTESIAN_POINT ( 'NONE',  ( -215.6254804987316334, 60.26473849368087343, 13.41209097274074047 ) ) ;
#5000 = LINE ( 'NONE', #280, #26518 ) ;
#5001 = DIRECTION ( 'NONE',  ( 0.000000000000000000, 0.000000000000000000, 1.000000000000000000 ) ) ;
#5002 = CARTESIAN_POINT ( 'NONE',  ( 79.99999999999991473, 80.00000000000001421, -100.0000000000000142 ) ) ;
#5003 = CARTESIAN_POINT ( 'NONE',  ( -223.0561610845317375, 88.57719356741800709, -14.95839461110579016 ) ) ;
#5004 = EDGE_CURVE ( 'NONE', #3825, #10017, #11465, .T. ) ;
#5005 = LINE ( 'NONE', #22399, #11979 ) ;
#5006 = CARTESIAN_POINT ( 'NONE',  ( 340.3127869742386338, 101.4626071723496779, -145.0000000000000000 ) ) ;
#5007 = CARTESIAN_POINT ( 'NONE',  ( 82.68942924499303615, 110.0997128786253683, 70.07812500014873081 ) ) ;
#5009 = CARTESIAN_POINT ( 'NONE',  ( -17.77354996712479007, 128.7458775741096133, 17.18687607546115004 ) ) ;
#5008 = VECTOR ( 'NONE', #2315, 1000.000000000000114 ) ;
#5010 = CARTESIAN_POINT ( 'NONE',  ( 232.4999999999996305, 83.06687458711267880, -36.86484227207694175 ) ) ;
#5011 = VECTOR ( 'NONE', #5846, 1000.000000000000000 ) ;
#5012 = LINE ( 'NONE', #11061, #8772 ) ;
#5013 = LINE ( 'NONE', #4725, #9308 ) ;
#5015 = VERTEX_POINT ( 'NONE', #18206 ) ;
#5014 = EDGE_LOOP ( 'NONE', ( #27583, #27170, #6085, #12182 ) ) ;
#5016 = CARTESIAN_POINT ( 'NONE',  ( -215.9971974014444811, 86.39790881275628465, -21.03121872006250825 ) ) ;
#5017 = VECTOR ( 'NONE', #24239, 1000.000000000000000 ) ;
#5018 = FACE_OUTER_BOUND ( 'NONE', #15674, .T. ) ;
#5019 = ORIENTED_EDGE ( 'NONE', *, *, #12839, .T. ) ;
#5020 = ORIENTED_EDGE ( 'NONE', *, *, #418, .T. ) ;
#5022 = ORIENTED_EDGE ( 'NONE', *, *, #5982, .T. ) ;
#5021 = CIRCLE ( 'NONE', #27487, 1.999999999999998224 ) ;
#5023 = CARTESIAN_POINT ( 'NONE',  ( 298.9233831825461039, 134.5963949001157687, -145.0000000000000000 ) ) ;
#5024 = DIRECTION ( 'NONE',  ( -0.000000000000000000, -0.000000000000000000, 1.000000000000000000 ) ) ;
#5025 = ORIENTED_EDGE ( 'NONE', *, *, #24924, .T. ) ;
#5026 = VERTEX_POINT ( 'NONE', #22657 ) ;
#5027 = DIRECTION ( 'NONE',  ( -1.387778780781444256E-14, -1.000000000000000000, 0.000000000000000000 ) ) ;
#5028 = CARTESIAN_POINT ( 'NONE',  ( 157.4999999999998579, 198.6830624361901414, 45.00000000000000000 ) ) ;
#5029 = AXIS2_PLACEMENT_3D ( 'NONE', #3004, #26708, #22408 ) ;
#5030 = FACE_OUTER_BOUND ( 'NONE', #13558, .T. ) ;
#5031 = ORIENTED_EDGE ( 'NONE', *, *, #486, .T. ) ;
#5032 = EDGE_CURVE ( 'NONE', #5806, #16800, #18347, .T. ) ;
#5033 = SURFACE_STYLE_FILL_AREA ( #24726 ) ;
#5034 = DIRECTION ( 'NONE',  ( 0.2383857661250380344, 0.9711705445023436356, 0.000000000000000000 ) ) ;
#5035 = EDGE_CURVE ( 'NONE', #20039, #14569, #4973, .T. ) ;
#5036 = VECTOR ( 'NONE', #23355, 1000.000000000000000 ) ;
#5037 = ADVANCED_FACE ( 'NONE', ( #2384 ), #25151, .F. ) ;
#5038 = FACE_OUTER_BOUND ( 'NONE', #8347, .T. ) ;
#5039 = CARTESIAN_POINT ( 'NONE',  ( -124.9781469243919076, 222.2250949724356985, -5.000000000000004441 ) ) ;
#5040 = CARTESIAN_POINT ( 'NONE',  ( -207.8278798888169945, 75.36218601466582356, -41.22349376586717540 ) ) ;
#5041 = DIRECTION ( 'NONE',  ( 1.000000000000000000, 0.000000000000000000, 0.000000000000000000 ) ) ;
#5042 = DIRECTION ( 'NONE',  ( 0.000000000000000000, 0.000000000000000000, -1.000000000000000000 ) ) ;
#5043 = DIRECTION ( 'NONE',  ( -0.000000000000000000, 0.000000000000000000, -1.000000000000000000 ) ) ;
#5044 = CARTESIAN_POINT ( 'NONE',  ( 217.4999999999996305, 83.06687458711267880, -36.86484227207694175 ) ) ;
#5045 = ORIENTED_EDGE ( 'NONE', *, *, #6467, .F. ) ;
#5046 = LINE ( 'NONE', #614, #6408 ) ;
#5047 = CARTESIAN_POINT ( 'NONE',  ( 367.4999999999996021, 44.41075299063184900, 1.850330238640837654E-14 ) ) ;
#5048 = LINE ( 'NONE', #19855, #10803 ) ;
#5049 = ORIENTED_EDGE ( 'NONE', *, *, #6093, .F. ) ;
#5050 =( LENGTH_UNIT ( ) NAMED_UNIT ( * ) SI_UNIT ( .MILLI., .METRE. ) );
#5051 = ORIENTED_EDGE ( 'NONE', *, *, #6001, .F. ) ;
#5052 = VECTOR ( 'NONE', #19381, 1000.000000000000000 ) ;
#5053 =( REPRESENTATION_RELATIONSHIP ('NONE','NONE', #11963, #10277 ) REPRESENTATION_RELATIONSHIP_WITH_TRANSFORMATION ( #8344 )SHAPE_REPRESENTATION_RELATIONSHIP( ) );
#5054 = DIRECTION ( 'NONE',  ( 0.000000000000000000, -1.000000000000000000, 0.000000000000000000 ) ) ;
#5055 = CARTESIAN_POINT ( 'NONE',  ( -175.0000000000000000, -120.0000000000001705, 70.00000000000001421 ) ) ;
#5056 = ORIENTED_EDGE ( 'NONE', *, *, #14671, .F. ) ;
#5057 = ADVANCED_BREP_SHAPE_REPRESENTATION ( '', ( #8800, #10637 ), #20272 ) ;
#5058 = ORIENTED_EDGE ( 'NONE', *, *, #24113, .F. ) ;
#5059 = DIRECTION ( 'NONE',  ( -1.000000000000000000, 0.000000000000000000, 0.000000000000000000 ) ) ;
#5060 = EDGE_CURVE ( 'NONE', #6335, #7010, #9008, .T. ) ;
#5061 = FACE_OUTER_BOUND ( 'NONE', #4560, .T. ) ;
#5062 = CARTESIAN_POINT ( 'NONE',  ( -216.6483861793289805, 139.2130420793173471, 15.04814241300593913 ) ) ;
#5063 = VERTEX_POINT ( 'NONE', #11316 ) ;
#5064 = DIRECTION ( 'NONE',  ( 0.000000000000000000, -0.000000000000000000, -1.000000000000000000 ) ) ;
#5065 = VERTEX_POINT ( 'NONE', #4682 ) ;
#5066 = DIRECTION ( 'NONE',  ( 0.4528218681382912836, -0.8916010070293483025, 0.000000000000000000 ) ) ;
#5067 = ADVANCED_FACE ( 'NONE', ( #13616 ), #24236, .T. ) ;
#5068 = VECTOR ( 'NONE', #17295, 1000.000000000000000 ) ;
#5069 = EDGE_CURVE ( 'NONE', #10866, #19795, #27095, .T. ) ;
#5070 = CARTESIAN_POINT ( 'NONE',  ( 158.0000000000010800, 103.1298746471690038, 45.00000000000000000 ) ) ;
#5071 = DIRECTION ( 'NONE',  ( -0.000000000000000000, 0.000000000000000000, -1.000000000000000000 ) ) ;
#5072 = CARTESIAN_POINT ( 'NONE',  ( 6.334507319946773407, 140.1911725318066715, -13.00000000064436634 ) ) ;
#5073 = LINE ( 'NONE', #15874, #26076 ) ;
#5074 = CARTESIAN_POINT ( 'NONE',  ( -262.5249090614869374, -166.4079007703013247, -89.92078834904907580 ) ) ;
#5075 = VECTOR ( 'NONE', #7807, 1000.000000000000114 ) ;
#5076 = DIRECTION ( 'NONE',  ( -0.000000000000000000, -0.000000000000000000, -1.000000000000000000 ) ) ;
#5077 = PRODUCT_RELATED_PRODUCT_CATEGORY ( 'part', '', ( #19210 ) ) ;
#5078 = EDGE_LOOP ( 'NONE', ( #10692, #15290, #14872, #333 ) ) ;
#5079 = CARTESIAN_POINT ( 'NONE',  ( 157.4999999999998579, 103.3838121509225090, 45.00000000000000000 ) ) ;
#5080 = DIRECTION ( 'NONE',  ( -1.000000000000000000, 0.000000000000000000, 0.000000000000000000 ) ) ;
#5081 = DIRECTION ( 'NONE',  ( -0.8916010070295820045, 0.4528218681378310406, 0.000000000000000000 ) ) ;
#5082 = CARTESIAN_POINT ( 'NONE',  ( -200.0000000000000284, -62.36067977499792647, 25.00000000000000000 ) ) ;
#5083 = ORIENTED_EDGE ( 'NONE', *, *, #22187, .F. ) ;
#5084 = DIRECTION ( 'NONE',  ( 1.000000000000000000, 0.000000000000000000, -0.000000000000000000 ) ) ;
#5085 = ORIENTED_EDGE ( 'NONE', *, *, #23141, .T. ) ;
#5086 = CARTESIAN_POINT ( 'NONE',  ( 79.99999999999992895, 240.0000000000000284, 5.000000000000002665 ) ) ;
#5087 = CARTESIAN_POINT ( 'NONE',  ( 157.4999999999997726, 246.3326875788235384, 45.00000000000000000 ) ) ;
#5088 = CARTESIAN_POINT ( 'NONE',  ( 138.0086035401004665, 249.8505569019347661, -150.2059422892478153 ) ) ;
#5089 = VERTEX_POINT ( 'NONE', #9583 ) ;
#5090 = CARTESIAN_POINT ( 'NONE',  ( 151.9705627484769650, 235.5563491861038017, -45.00000000000000000 ) ) ;
#5091 = DIRECTION ( 'NONE',  ( -1.000000000000000000, 0.000000000000000000, 0.000000000000000000 ) ) ;
#5092 = ORIENTED_EDGE ( 'NONE', *, *, #3991, .T. ) ;
#5093 = CIRCLE ( 'NONE', #20678, 6.025000000000002132 ) ;
#5094 = CARTESIAN_POINT ( 'NONE',  ( -62.69330818947670281, 133.3645688629142967, 15.73244652714148373 ) ) ;
#5095 = VERTEX_POINT ( 'NONE', #2816 ) ;
#5096 = CARTESIAN_POINT ( 'NONE',  ( 157.4999999999994884, 211.2224374737238577, 45.00000000000000000 ) ) ;
#5097 = EDGE_LOOP ( 'NONE', ( #23585, #24538, #1561, #3389 ) ) ;
#5098 = EDGE_CURVE ( 'NONE', #2906, #24273, #20206, .T. ) ;
#5099 = VERTEX_POINT ( 'NONE', #7426 ) ;
#5100 = CARTESIAN_POINT ( 'NONE',  ( 179.9999999999999147, -5.589247009368164321, 100.0000000000000142 ) ) ;
#5101 = EDGE_LOOP ( 'NONE', ( #27031, #15018, #23939, #19051 ) ) ;
#5102 = ADVANCED_FACE ( 'NONE', ( #15627 ), #7284, .T. ) ;
#5103 = ORIENTED_EDGE ( 'NONE', *, *, #6236, .T. ) ;
#5104 = ORIENTED_EDGE ( 'NONE', *, *, #22981, .T. ) ;
#5105 = CARTESIAN_POINT ( 'NONE',  ( 158.0000000000002842, 178.8739998798873216, 45.00000000000000000 ) ) ;
#5106 = ADVANCED_FACE ( 'NONE', ( #15917 ), #24664, .F. ) ;
#5107 = PLANE ( 'NONE',  #1594 ) ;
#5108 = DIRECTION ( 'NONE',  ( 1.000000000000000000, 0.000000000000000000, 0.000000000000000000 ) ) ;
#5109 = DIRECTION ( 'NONE',  ( -0.9784193629480781862, 0.2066290158914688424, 0.000000000000000000 ) ) ;
#5110 = DIRECTION ( 'NONE',  ( 0.000000000000000000, -1.000000000000000000, 0.000000000000000000 ) ) ;
#5111 = CARTESIAN_POINT ( 'NONE',  ( 118.0294372515228787, 204.4436508138956015, 45.00000000000000000 ) ) ;
#5112 = EDGE_CURVE ( 'NONE', #13671, #25239, #1091, .T. ) ;
#5113 = VECTOR ( 'NONE', #18482, 1000.000000000000000 ) ;
#5114 = DIRECTION ( 'NONE',  ( -0.000000000000000000, -0.000000000000000000, 1.000000000000000000 ) ) ;
#5115 = CARTESIAN_POINT ( 'NONE',  ( 217.4999999999996305, -5.589247009368136787, -100.0000000000000142 ) ) ;
#5116 = CARTESIAN_POINT ( 'NONE',  ( -279.1278187736259611, -170.0000000000001421, 106.1966075482099683 ) ) ;
#5117 = DIRECTION ( 'NONE',  ( -0.000000000000000000, -0.000000000000000000, 1.000000000000000000 ) ) ;
#5118 = LINE ( 'NONE', #11166, #6125 ) ;
#5119 = PRESENTATION_LAYER_ASSIGNMENT (  '', '', ( #7428 ) ) ;
#5120 = ORIENTED_EDGE ( 'NONE', *, *, #13622, .F. ) ;
#5121 = CYLINDRICAL_SURFACE ( 'NONE', #22970, 30.00000000000000000 ) ;
#5122 = AXIS2_PLACEMENT_3D ( 'NONE', #4835, #22372, #2683 ) ;
#5123 = CARTESIAN_POINT ( 'NONE',  ( 155.4185842870419947, 230.6339745962152392, 45.00000000000000000 ) ) ;
#5124 = CARTESIAN_POINT ( 'NONE',  ( 162.0806940948679085, 180.4841764145329250, 45.00000000000000000 ) ) ;
#5125 = CARTESIAN_POINT ( 'NONE',  ( 157.9999999999998863, 216.4921249924925348, 45.00000000000000000 ) ) ;
#5126 = ORIENTED_EDGE ( 'NONE', *, *, #11746, .T. ) ;
#5127 = AXIS2_PLACEMENT_3D ( 'NONE', #27053, #14140, #5221 ) ;
#5128 = EDGE_CURVE ( 'NONE', #1940, #12493, #21033, .T. ) ;
#5129 = DIRECTION ( 'NONE',  ( 0.4528218681372721544, 0.8916010070298658885, -0.000000000000000000 ) ) ;
#5130 = ORIENTED_EDGE ( 'NONE', *, *, #11875, .F. ) ;
#5131 = CARTESIAN_POINT ( 'NONE',  ( -141.6428522700808230, 69.54464929955099706, 83.00000000000001421 ) ) ;
#5132 = ORIENTED_EDGE ( 'NONE', *, *, #28205, .F. ) ;
#5133 = ADVANCED_FACE ( 'NONE', ( #27364 ), #11411, .T. ) ;
#5134 = VECTOR ( 'NONE', #10708, 1000.000000000000000 ) ;
#5135 = ORIENTED_EDGE ( 'NONE', *, *, #19792, .T. ) ;
#5136 = ORIENTED_EDGE ( 'NONE', *, *, #7953, .F. ) ;
#5137 = ORIENTED_EDGE ( 'NONE', *, *, #24717, .T. ) ;
#5138 = CARTESIAN_POINT ( 'NONE',  ( -138.8850951481510378, 128.5925778606047061, 15.90076932754394612 ) ) ;
#5139 = AXIS2_PLACEMENT_3D ( 'NONE', #14395, #16687, #14117 ) ;
#5140 = CARTESIAN_POINT ( 'NONE',  ( -110.3221550338875687, 68.51688903468615877, 83.00000000000001421 ) ) ;
#5141 = LINE ( 'NONE', #271, #5620 ) ;
#5142 = VECTOR ( 'NONE', #14747, 1000.000000000000114 ) ;
#5143 = CARTESIAN_POINT ( 'NONE',  ( -107.9388568470210856, 135.2304614929108482, -15.33442335600818396 ) ) ;
#5144 = UNCERTAINTY_MEASURE_WITH_UNIT (LENGTH_MEASURE( 1.000000000000000082E-05 ), #26485, 'distance_accuracy_value', 'NONE');
#5145 = DIRECTION ( 'NONE',  ( 1.000000000000000000, 0.000000000000000000, -0.000000000000000000 ) ) ;
#5146 = EDGE_CURVE ( 'NONE', #16800, #12640, #24714, .T. ) ;
#5147 = CARTESIAN_POINT ( 'NONE',  ( -207.7463451706791773, 75.42136631982602069, 41.72512927420302020 ) ) ;
#5148 = DIRECTION ( 'NONE',  ( 0.8916010070298252543, -0.4528218681373520904, 0.000000000000000000 ) ) ;
#5149 = DIRECTION ( 'NONE',  ( 0.000000000000000000, 0.000000000000000000, -1.000000000000000000 ) ) ;
#5150 = EDGE_CURVE ( 'NONE', #14154, #5759, #19511, .T. ) ;
#5151 = CARTESIAN_POINT ( 'NONE',  ( 79.99999999999995737, 109.8066173636171499, -73.92694226569399518 ) ) ;
#5152 = FACE_OUTER_BOUND ( 'NONE', #6286, .T. ) ;
#5153 =( NAMED_UNIT ( * ) SI_UNIT ( $, .STERADIAN. ) SOLID_ANGLE_UNIT ( ) );
#5154 = DIRECTION ( 'NONE',  ( 1.000000000000000000, 0.000000000000000000, 0.000000000000000000 ) ) ;
#5155 = CARTESIAN_POINT ( 'NONE',  ( 109.9999999999999147, 137.0808454111986237, 89.99999999939370809 ) ) ;
#5156 = AXIS2_PLACEMENT_3D ( 'NONE', #7372, #12115, #3045 ) ;
#5157 = AXIS2_PLACEMENT_3D ( 'NONE', #15697, #10951, #13397 ) ;
#5158 = FACE_OUTER_BOUND ( 'NONE', #325, .T. ) ;
#5159 = CARTESIAN_POINT ( 'NONE',  ( 133.9999999999998295, 242.9999999999997158, 45.00000000000000000 ) ) ;
#5160 = DIRECTION ( 'NONE',  ( -0.7440215159219069063, -0.6681556583950086781, 0.000000000000000000 ) ) ;
#5161 = VECTOR ( 'NONE', #4964, 1000.000000000000000 ) ;
#5163 = EDGE_LOOP ( 'NONE', ( #20366, #23723, #15792 ) ) ;
#5162 = ORIENTED_EDGE ( 'NONE', *, *, #4227, .F. ) ;
#5164 = EDGE_CURVE ( 'NONE', #1242, #19224, #19661, .T. ) ;
#5165 = CARTESIAN_POINT ( 'NONE',  ( -220.6963704969327011, 86.29915981945389092, -18.37871326271141115 ) ) ;
#5166 = AXIS2_PLACEMENT_3D ( 'NONE', #25267, #12218, #18803 ) ;
#5167 = LINE ( 'NONE', #19436, #20295 ) ;
#5168 = ORIENTED_EDGE ( 'NONE', *, *, #7787, .T. ) ;
#5170 = EDGE_CURVE ( 'NONE', #16458, #14195, #16752, .T. ) ;
#5169 = VERTEX_POINT ( 'NONE', #7573 ) ;
#5171 = DIRECTION ( 'NONE',  ( -0.000000000000000000, -0.000000000000000000, -1.000000000000000000 ) ) ;
#5172 = CARTESIAN_POINT ( 'NONE',  ( -122.5470052484187704, 131.3754805985278438, 16.25370679815316066 ) ) ;
#5173 = ORIENTED_EDGE ( 'NONE', *, *, #9225, .T. ) ;
#5174 = EDGE_CURVE ( 'NONE', #7228, #16274, #14595, .T. ) ;
#5175 = ORIENTED_EDGE ( 'NONE', *, *, #15329, .T. ) ;
#5176 = FACE_OUTER_BOUND ( 'NONE', #3288, .T. ) ;
#5177 = AXIS2_PLACEMENT_3D ( 'NONE', #21215, #12756, #1537 ) ;
#5178 = DIRECTION ( 'NONE',  ( -0.000000000000000000, -0.000000000000000000, -1.000000000000000000 ) ) ;
#5179 = VECTOR ( 'NONE', #24987, 1000.000000000000000 ) ;
#5180 = DIRECTION ( 'NONE',  ( 0.000000000000000000, 0.000000000000000000, -1.000000000000000000 ) ) ;
#5181 = AXIS2_PLACEMENT_3D ( 'NONE', #17946, #22254, #19954 ) ;
#5182 = CARTESIAN_POINT ( 'NONE',  ( 157.4999999999998579, 188.6515624061619576, -45.00000000000000000 ) ) ;
#5183 = VECTOR ( 'NONE', #14605, 1000.000000000000000 ) ;
#5184 = LINE ( 'NONE', #27289, #4793 ) ;
#5185 = DIRECTION ( 'NONE',  ( 0.8916010070300285362, 0.4528218681369517995, 0.000000000000000000 ) ) ;
#5186 = CARTESIAN_POINT ( 'NONE',  ( -209.7310389751728508, 59.98715598645322444, -17.47553936829965338 ) ) ;
#5187 = DIRECTION ( 'NONE',  ( -0.8916010070291696676, -0.4528218681386429467, 0.000000000000000000 ) ) ;
#5188 = FACE_OUTER_BOUND ( 'NONE', #28258, .T. ) ;
#5189 = DIRECTION ( 'NONE',  ( 0.8916010070293783896, -0.4528218681382319422, 0.000000000000000000 ) ) ;
#5190 = LINE ( 'NONE', #27431, #2476 ) ;
#5191 = ORIENTED_EDGE ( 'NONE', *, *, #25877, .T. ) ;
#5192 = DIRECTION ( 'NONE',  ( 1.000000000000000000, -0.000000000000000000, -0.000000000000000000 ) ) ;
#5193 = VECTOR ( 'NONE', #6498, 1000.000000000000227 ) ;
#5194 = CARTESIAN_POINT ( 'NONE',  ( -235.5733620266476578, 80.43390826602548316, 15.03591609561660469 ) ) ;
#5195 = DIRECTION ( 'NONE',  ( -0.000000000000000000, -0.000000000000000000, -1.000000000000000000 ) ) ;
#5196 = VERTEX_POINT ( 'NONE', #11890 ) ;
#5197 =( NAMED_UNIT ( * ) PLANE_ANGLE_UNIT ( ) SI_UNIT ( $, .RADIAN. ) );
#5198 = VECTOR ( 'NONE', #18654, 1000.000000000000000 ) ;
#5200 = ORIENTED_EDGE ( 'NONE', *, *, #22259, .T. ) ;
#5199 = ADVANCED_FACE ( 'NONE', ( #16472 ), #16894, .T. ) ;
#5201 = EDGE_CURVE ( 'NONE', #10815, #14295, #10283, .T. ) ;
#5202 = DIRECTION ( 'NONE',  ( -0.000000000000000000, -0.000000000000000000, -1.000000000000000000 ) ) ;
#5203 = EDGE_LOOP ( 'NONE', ( #24503, #8433, #19334, #516 ) ) ;
#5204 = VERTEX_POINT ( 'NONE', #7839 ) ;
#5205 = DIRECTION ( 'NONE',  ( 1.000000000000000000, 0.000000000000000000, 0.000000000000000000 ) ) ;
#5206 = CARTESIAN_POINT ( 'NONE',  ( 135.1062353973271968, 7.258260926501912458, 45.00000000000000000 ) ) ;
#5207 = CARTESIAN_POINT ( 'NONE',  ( 65.00000000000000000, -120.0000000000000711, 76.00000000000001421 ) ) ;
#5208 = ORIENTED_EDGE ( 'NONE', *, *, #22819, .F. ) ;
#5209 = DIRECTION ( 'NONE',  ( 0.000000000000000000, -1.000000000000000000, 0.000000000000000000 ) ) ;
#5210 = ORIENTED_EDGE ( 'NONE', *, *, #13674, .T. ) ;
#5211 = VECTOR ( 'NONE', #15544, 1000.000000000000000 ) ;
#5212 = CARTESIAN_POINT ( 'NONE',  ( 158.0000000000017337, 42.94087446699998623, -45.00000000000000000 ) ) ;
#5213 = VECTOR ( 'NONE', #4211, 1000.000000000000000 ) ;
#5214 = EDGE_CURVE ( 'NONE', #19703, #15612, #27645, .T. ) ;
#5215 = DIRECTION ( 'NONE',  ( -0.000000000000000000, -0.000000000000000000, -1.000000000000000000 ) ) ;
#5216 = DIRECTION ( 'NONE',  ( 0.8916010070293783896, -0.4528218681382319422, 0.000000000000000000 ) ) ;
#5217 = CARTESIAN_POINT ( 'NONE',  ( -25.41071799330663694, 129.2224460950298237, -15.66088409790421920 ) ) ;
#5218 = VECTOR ( 'NONE', #7948, 1000.000000000000000 ) ;
#5219 = DIRECTION ( 'NONE',  ( 0.4528218681375906218, -0.8916010070297041290, 0.000000000000000000 ) ) ;
#5220 = DIRECTION ( 'NONE',  ( 0.8916010070296531698, -0.4528218681376911525, 0.000000000000000000 ) ) ;
#5221 = DIRECTION ( 'NONE',  ( -0.8916010070298862056, 0.4528218681372321863, 0.000000000000000000 ) ) ;
#5222 = ORIENTED_EDGE ( 'NONE', *, *, #6943, .F. ) ;
#5223 = EDGE_CURVE ( 'NONE', #18214, #19744, #5687, .T. ) ;
#5224 = CYLINDRICAL_SURFACE ( 'NONE', #21940, 5.999999999999991118 ) ;
#5225 = DIRECTION ( 'NONE',  ( 0.000000000000000000, 0.000000000000000000, -1.000000000000000000 ) ) ;
#5226 = CARTESIAN_POINT ( 'NONE',  ( 158.0000000000003979, 168.8424998498591663, 45.00000000000000000 ) ) ;
#5227 = FACE_OUTER_BOUND ( 'NONE', #23456, .T. ) ;
#5228 = ORIENTED_EDGE ( 'NONE', *, *, #21351, .T. ) ;
#5229 = CARTESIAN_POINT ( 'NONE',  ( -231.1953787138146765, 65.04295872140690449, 6.836033801457080727 ) ) ;
#5230 = VERTEX_POINT ( 'NONE', #7982 ) ;
#5231 = DIRECTION ( 'NONE',  ( 1.000000000000000000, 0.000000000000000000, 0.000000000000000000 ) ) ;
#5232 = CARTESIAN_POINT ( 'NONE',  ( -220.3653290071072206, 61.04242272473436515, -10.83006322850141778 ) ) ;
#5233 = CARTESIAN_POINT ( 'NONE',  ( 135.3925546936119417, 249.9980781680236532, -139.0095862629495116 ) ) ;
#5234 = EDGE_LOOP ( 'NONE', ( #27799, #10042 ) ) ;
#5235 = LINE ( 'NONE', #653, #2818 ) ;
#5236 = CARTESIAN_POINT ( 'NONE',  ( -146.6428522700808230, 22.24192588826928585, 80.00000000000001421 ) ) ;
#5237 = EDGE_CURVE ( 'NONE', #1480, #19459, #23351, .T. ) ;
#5238 = EDGE_LOOP ( 'NONE', ( #1910, #26945, #17264 ) ) ;
#5239 = VECTOR ( 'NONE', #19731, 1000.000000000000000 ) ;
#5240 = EDGE_CURVE ( 'NONE', #28016, #27342, #25222, .T. ) ;
#5241 = DIRECTION ( 'NONE',  ( 0.000000000000000000, 1.000000000000000000, 1.214306433183764966E-16 ) ) ;
#5242 = EDGE_CURVE ( 'NONE', #502, #26105, #953, .T. ) ;
#5243 = CARTESIAN_POINT ( 'NONE',  ( 97.02590988242761227, 241.2701841432802041, 10.66915916737285031 ) ) ;
#5244 = ORIENTED_EDGE ( 'NONE', *, *, #24325, .T. ) ;
#5245 = VECTOR ( 'NONE', #22438, 1000.000000000000000 ) ;
#5246 = ORIENTED_EDGE ( 'NONE', *, *, #20910, .T. ) ;
#5247 = DIRECTION ( 'NONE',  ( -0.000000000000000000, 0.000000000000000000, -1.000000000000000000 ) ) ;
#5248 = VERTEX_POINT ( 'NONE', #27232 ) ;
#5249 = ORIENTED_EDGE ( 'NONE', *, *, #84, .T. ) ;
#5250 = ORIENTED_EDGE ( 'NONE', *, *, #17544, .F. ) ;
#5251 = CARTESIAN_POINT ( 'NONE',  ( 107.7175597583454021, 250.4128021203281946, 33.27520275799354010 ) ) ;
#5252 = VECTOR ( 'NONE', #1001, 1000.000000000000000 ) ;
#5253 = DIRECTION ( 'NONE',  ( 0.000000000000000000, 0.000000000000000000, 1.000000000000000000 ) ) ;
#5254 = CARTESIAN_POINT ( 'NONE',  ( 79.99999999999994316, -70.00000000000002842, 100.0000000000000142 ) ) ;
#5255 = VECTOR ( 'NONE', #25733, 1000.000000000000114 ) ;
#5256 = CARTESIAN_POINT ( 'NONE',  ( 101.7779539750033280, 119.2876405404464890, -82.50000000032424907 ) ) ;
#5257 = DIRECTION ( 'NONE',  ( -1.000000000000000000, 0.000000000000000000, -0.000000000000000000 ) ) ;
#5258 = DIRECTION ( 'NONE',  ( -0.8916010070293384215, 0.4528218681383106015, 0.000000000000000000 ) ) ;
#5259 = DIRECTION ( 'NONE',  ( 0.8018642810807398158, 0.5975062131282554700, -0.000000000000000000 ) ) ;
#5260 = DIRECTION ( 'NONE',  ( 0.000000000000000000, -1.000000000000000000, 0.000000000000000000 ) ) ;
#5261 = AXIS2_PLACEMENT_3D ( 'NONE', #17632, #28252, #25824 ) ;
#5262 = LINE ( 'NONE', #7706, #6028 ) ;
#5263 = DIRECTION ( 'NONE',  ( 0.000000000000000000, 0.000000000000000000, -1.000000000000000000 ) ) ;
#5264 = CARTESIAN_POINT ( 'NONE',  ( 115.6411010564591777, 208.5333949359988139, -99.00000000000001421 ) ) ;
#5265 = ORIENTED_EDGE ( 'NONE', *, *, #25795, .T. ) ;
#5266 = EDGE_CURVE ( 'NONE', #3350, #19969, #16337, .T. ) ;
#5267 = ADVANCED_FACE ( 'NONE', ( #20770 ), #22933, .F. ) ;
#5268 = EDGE_CURVE ( 'NONE', #5960, #11012, #9607, .T. ) ;
#5269 = CARTESIAN_POINT ( 'NONE',  ( 158.0000000000004547, 163.8267498348450886, 45.00000000000000000 ) ) ;
#5270 = DIRECTION ( 'NONE',  ( -0.8916010070295314893, -0.4528218681379303501, 0.000000000000000000 ) ) ;
#5271 = LINE ( 'NONE', #14056, #10621 ) ;
#5272 = VERTEX_POINT ( 'NONE', #15168 ) ;
#5273 = LINE ( 'NONE', #9734, #18944 ) ;
#5274 = ORIENTED_EDGE ( 'NONE', *, *, #13093, .F. ) ;
#5275 = EDGE_CURVE ( 'NONE', #12260, #15470, #5914, .T. ) ;
#5276 = FILL_AREA_STYLE ('',( #9597 ) ) ;
#5277 = VECTOR ( 'NONE', #21179, 1000.000000000000000 ) ;
#5278 = CIRCLE ( 'NONE', #3889, 4.355764593064429313 ) ;
#5279 = ORIENTED_EDGE ( 'NONE', *, *, #10174, .T. ) ;
#5280 = VERTEX_POINT ( 'NONE', #17022 ) ;
#5281 = VERTEX_POINT ( 'NONE', #17443 ) ;
#5282 = AXIS2_PLACEMENT_3D ( 'NONE', #26032, #21735, #16860 ) ;
#5283 = EDGE_LOOP ( 'NONE', ( #2288, #13556, #20817, #3682 ) ) ;
#5284 = CARTESIAN_POINT ( 'NONE',  ( -75.07674457730871609, 136.1111122117180798, 13.54517443609203653 ) ) ;
#5285 = CARTESIAN_POINT ( 'NONE',  ( 150.8670668058247202, 207.8247714198255949, -45.00000000000000000 ) ) ;
#5286 = CARTESIAN_POINT ( 'NONE',  ( 109.9999999999999432, 2.035408878479452500E-14, 100.0000000000000142 ) ) ;
#5287 = CARTESIAN_POINT ( 'NONE',  ( -42.65532241761712839, 131.0044336801081784, -16.34779397420837910 ) ) ;
#5288 = CARTESIAN_POINT ( 'NONE',  ( -18.10916961908506551, 129.9686900844010893, 15.33252739753482885 ) ) ;
#5289 = CARTESIAN_POINT ( 'NONE',  ( -207.5064340660269693, 75.59749780642115979, 45.29313139209890693 ) ) ;
#5290 = CARTESIAN_POINT ( 'NONE',  ( 79.99999999999994316, -100.0000000000000284, 25.00000000000000711 ) ) ;
#5291 = CARTESIAN_POINT ( 'NONE',  ( -59.48697296830715686, 2.336311854928213219E-15, 100.0000000000000000 ) ) ;
#5292 = DIRECTION ( 'NONE',  ( 1.000000000000000000, 0.000000000000000000, 0.000000000000000000 ) ) ;
#5293 = VECTOR ( 'NONE', #16010, 1000.000000000000000 ) ;
#5294 = CARTESIAN_POINT ( 'NONE',  ( -211.7690755206428719, 88.48850965457344842, -21.98930932911726899 ) ) ;
#5295 = DIRECTION ( 'NONE',  ( -0.000000000000000000, -0.000000000000000000, 1.000000000000000000 ) ) ;
#5296 = DIRECTION ( 'NONE',  ( -0.8660254037844363761, 0.5000000000000041078, -0.000000000000000000 ) ) ;
#5297 = DIRECTION ( 'NONE',  ( -1.000000000000000000, 0.000000000000000000, 0.000000000000000000 ) ) ;
#5298 = VECTOR ( 'NONE', #19213, 1000.000000000000000 ) ;
#5299 = EDGE_CURVE ( 'NONE', #23283, #9810, #12731, .T. ) ;
#5300 = EDGE_CURVE ( 'NONE', #7257, #366, #8193, .T. ) ;
#5301 = CARTESIAN_POINT ( 'NONE',  ( 158.0000000000014211, 73.03537455708450921, 45.00000000000000000 ) ) ;
#5302 = CARTESIAN_POINT ( 'NONE',  ( -192.4056874188291602, 101.4351547665440023, 32.80394979098671371 ) ) ;
#5303 = DIRECTION ( 'NONE',  ( 0.000000000000000000, 0.000000000000000000, 1.000000000000000000 ) ) ;
#5304 = VECTOR ( 'NONE', #14957, 1000.000000000000227 ) ;
#5306 = ORIENTED_EDGE ( 'NONE', *, *, #17384, .T. ) ;
#5305 = ORIENTED_EDGE ( 'NONE', *, *, #22027, .F. ) ;
#5307 = PLANE ( 'NONE',  #580 ) ;
#5308 = VERTEX_POINT ( 'NONE', #6387 ) ;
#5309 = VERTEX_POINT ( 'NONE', #12871 ) ;
#5310 = ADVANCED_FACE ( 'NONE', ( #21764 ), #10969, .F. ) ;
#5311 = FACE_OUTER_BOUND ( 'NONE', #5646, .T. ) ;
#5312 = EDGE_CURVE ( 'NONE', #5313, #13707, #23636, .T. ) ;
#5313 = VERTEX_POINT ( 'NONE', #10990 ) ;
#5314 = VECTOR ( 'NONE', #8613, 1000.000000000000000 ) ;
#5315 = EDGE_LOOP ( 'NONE', ( #25611, #3271, #28290, #4765 ) ) ;
#5316 = CARTESIAN_POINT ( 'NONE',  ( 232.4999999999996305, 83.06687458711267880, -36.86484227207694175 ) ) ;
#5317 = VECTOR ( 'NONE', #11866, 1000.000000000000000 ) ;
#5318 = CARTESIAN_POINT ( 'NONE',  ( -17.24491960465745777, -18.01420295945611727, 80.00000000000001421 ) ) ;
#5319 = DIRECTION ( 'NONE',  ( -0.000000000000000000, -0.000000000000000000, -1.000000000000000000 ) ) ;
#5320 =( BOUNDED_SURFACE ( )  B_SPLINE_SURFACE ( 3, 2, ( 
 ( #25811, #14913, #28097 ),
 ( #5714, #1401, #23667 ),
 ( #3973, #12760, #6276 ),
 ( #21500, #15050, #19495 ),
 ( #17332, #12340, #1818 ),
 ( #10173, #10592, #28239 ),
 ( #19348, #3547, #12901 ),
 ( #21648, #1958, #14488 ),
 ( #23245, #16779, #18930 ),
 ( #27673, #8013, #13463 ),
 ( #11459, #15195, #15482 ),
 ( #9003, #23952, #22072 ) ),
 .UNSPECIFIED., .F., .F., .F. ) 
 B_SPLINE_SURFACE_WITH_KNOTS ( ( 4, 2, 2, 2, 2, 4 ),
 ( 3, 3 ),
 ( 0.000000000000000000, 0.004509302159734392135, 0.009018604319468784269, 0.01127325539933598034, 0.01352790647920317640, 0.01803720863893756854 ),
 ( 0.000000000000000000, 1.000000000000000000 ),
 .UNSPECIFIED. ) 
 GEOMETRIC_REPRESENTATION_ITEM ( )  RATIONAL_B_SPLINE_SURFACE ( (
 ( 1.000000000000000000, 0.7071067811865475727, 1.000000000000000000),
 ( 1.000000000000000000, 0.7035406144708270526, 1.000000000000000000),
 ( 1.000000000000000000, 0.7008848705186870864, 1.000000000000000000),
 ( 1.000000000000000000, 0.6974083274405008526, 1.000000000000000000),
 ( 1.000000000000000000, 0.6965884901777600335, 1.000000000000000000),
 ( 1.000000000000000000, 0.6967133934288484154, 1.000000000000000000),
 ( 1.000000000000000000, 0.6969819717335956621, 1.000000000000000000),
 ( 1.000000000000000000, 0.6979534373899805022, 1.000000000000000000),
 ( 1.000000000000000000, 0.6986531993633946502, 1.000000000000000000),
 ( 1.000000000000000000, 0.7013382012354564266, 1.000000000000000000),
 ( 1.000000000000000000, 0.7039093929050953546, 1.000000000000000000),
 ( 1.000000000000000000, 0.7071067811865475727, 1.000000000000000000) ) ) 
 REPRESENTATION_ITEM ( '' )  SURFACE ( )  );
#5321 = VECTOR ( 'NONE', #7664, 1000.000000000000000 ) ;
#5322 = CARTESIAN_POINT ( 'NONE',  ( 93.83233610022676885, 231.2056637020306198, -18.37429547533238861 ) ) ;
#5323 = EDGE_CURVE ( 'NONE', #28009, #20034, #10422, .T. ) ;
#5324 = ADVANCED_FACE ( 'NONE', ( #64 ), #17585, .F. ) ;
#5325 = DIRECTION ( 'NONE',  ( 0.4528218681382713551, 0.8916010070293584056, -0.000000000000000000 ) ) ;
#5326 = CARTESIAN_POINT ( 'NONE',  ( 158.0000000000001137, 195.9212499249295831, 45.00000000000000000 ) ) ;
#5327 = CARTESIAN_POINT ( 'NONE',  ( -221.9864287755668784, 60.98533040124252835, -21.67821222923991442 ) ) ;
#5328 = CARTESIAN_POINT ( 'NONE',  ( 109.9999999999999005, 230.0000000000000284, -5.000000000000004441 ) ) ;
#5329 = CARTESIAN_POINT ( 'NONE',  ( 157.4999999999998579, 108.3995621659365867, 45.00000000000000000 ) ) ;
#5330 = DIRECTION ( 'NONE',  ( 0.4528218681376512400, 0.8916010070296733758, -0.000000000000000000 ) ) ;
#5331 = CARTESIAN_POINT ( 'NONE',  ( 192.5108452903457419, 172.8810361401565672, 45.00000000000000000 ) ) ;
#5332 = ORIENTED_EDGE ( 'NONE', *, *, #12122, .F. ) ;
#5333 = VECTOR ( 'NONE', #25721, 1000.000000000000114 ) ;
#5334 = DIRECTION ( 'NONE',  ( 0.8916010070293584056, -0.4528218681382712996, 0.000000000000000000 ) ) ;
#5335 = CARTESIAN_POINT ( 'NONE',  ( -239.6893155506737401, 70.91029463950323475, 5.253362301622646946 ) ) ;
#5336 = LINE ( 'NONE', #16544, #26391 ) ;
#5337 = VERTEX_POINT ( 'NONE', #15021 ) ;
#5338 = DIRECTION ( 'NONE',  ( 0.000000000000000000, 0.000000000000000000, 0.9999999999999998890 ) ) ;
#5339 = CIRCLE ( 'NONE', #3036, 75.00000000000002842 ) ;
#5340 = B_SPLINE_CURVE_WITH_KNOTS ( 'NONE', 3,
 ( #789, #505, #24491, #24341, #9557, #13300, #13877, #22336, #5088, #4800, #2354, #22630, #9268, #4939, #13439, #22193, #11137, #9120, #26482, #17735, #6956, #9416, #11579, #6813, #13733, #2788, #15598, #4651, #2497, #11287, #26633, #13587, #2646, #651, #20177, #26788, #18177, #26931, #7679, #3212, #10118, #5233, #20739, #11998 ),
 .UNSPECIFIED., .F., .F.,
 ( 4, 2, 2, 2, 2, 2, 2, 2, 2, 2, 2, 2, 2, 2, 2, 2, 2, 2, 2, 2, 2, 4 ),
 ( 2.775557561562891351E-17, 0.001175389346958573842, 0.001763084020437806227, 0.002350778693917038829, 0.003526168040875585132, 0.004701557387834132302, 0.005876946734792679039, 0.007052336081751224908, 0.007640030755230537741, 0.008227725428709848840, 0.009403114775668379097, 0.01057850412262690762, 0.01175389346958543614, 0.01234158814306466484, 0.01292928281654389007, 0.01410467216350234400, 0.01528006151046080140, 0.01586775618394002663, 0.01645545085741925359, 0.01763084020437779079, 0.01821853487785705938, 0.01880622955133632798 ),
 .UNSPECIFIED. ) ;
#5341 = ORIENTED_EDGE ( 'NONE', *, *, #26487, .T. ) ;
#5342 = EDGE_CURVE ( 'NONE', #15188, #23617, #9124, .T. ) ;
#5343 = CARTESIAN_POINT ( 'NONE',  ( 105.2480867105129505, 123.6573351778161793, 100.0000000000216573 ) ) ;
#5344 = CARTESIAN_POINT ( 'NONE',  ( 157.9999999999999432, 213.4763749774776045, 45.00000000000000000 ) ) ;
#5345 = ORIENTED_EDGE ( 'NONE', *, *, #1095, .F. ) ;
#5346 = VERTEX_POINT ( 'NONE', #8409 ) ;
#5347 = LINE ( 'NONE', #9094, #6274 ) ;
#5348 = CARTESIAN_POINT ( 'NONE',  ( 157.4999999999998579, 95.86018712840139244, -45.00000000000000000 ) ) ;
#5349 = CARTESIAN_POINT ( 'NONE',  ( 216.4313787033304379, 124.9567147554451623, 45.00000000000000000 ) ) ;
#5350 = ORIENTED_EDGE ( 'NONE', *, *, #8213, .F. ) ;
#5351 = CARTESIAN_POINT ( 'NONE',  ( 158.0000000000011653, 93.60624962464788723, 45.00000000000000000 ) ) ;
#5352 = VERTEX_POINT ( 'NONE', #8269 ) ;
#5353 = DIRECTION ( 'NONE',  ( -0.000000000000000000, 0.000000000000000000, -1.000000000000000000 ) ) ;
#5354 = DIRECTION ( 'NONE',  ( 0.4528218681383106015, -0.8916010070293384215, 0.000000000000000000 ) ) ;
#5355 = CARTESIAN_POINT ( 'NONE',  ( 157.4999999999996305, 283.9508126914284958, 45.00000000000000000 ) ) ;
#5356 = CARTESIAN_POINT ( 'NONE',  ( 4.595825946142663376, 138.9899071332870335, -14.95390936462971254 ) ) ;
#5357 = DIRECTION ( 'NONE',  ( 0.000000000000000000, 0.000000000000000000, 1.000000000000000000 ) ) ;
#5358 = EDGE_CURVE ( 'NONE', #1242, #19844, #20581, .T. ) ;
#5359 = EDGE_CURVE ( 'NONE', #1908, #1347, #6529, .T. ) ;
#5360 = LINE ( 'NONE', #27193, #24321 ) ;
#5361 = FACE_OUTER_BOUND ( 'NONE', #6248, .T. ) ;
#5362 = EDGE_LOOP ( 'NONE', ( #1496, #23892, #16217, #10021 ) ) ;
#5363 = CARTESIAN_POINT ( 'NONE',  ( 157.9999999999997442, 251.6023750975910218, 45.00000000000000000 ) ) ;
#5364 = EDGE_CURVE ( 'NONE', #12131, #4224, #18322, .T. ) ;
#5365 = LINE ( 'NONE', #13723, #16606 ) ;
#5366 = DIRECTION ( 'NONE',  ( -0.000000000000000000, -0.000000000000000000, -1.000000000000000000 ) ) ;
#5367 = ORIENTED_EDGE ( 'NONE', *, *, #7288, .F. ) ;
#5368 = DIRECTION ( 'NONE',  ( -1.000000000000000000, -2.602085213965211135E-16, 0.000000000000000000 ) ) ;
#5369 = ORIENTED_EDGE ( 'NONE', *, *, #19830, .T. ) ;
#5370 = DIRECTION ( 'NONE',  ( 0.000000000000000000, 0.000000000000000000, -1.000000000000000000 ) ) ;
#5371 = PLANE ( 'NONE',  #10113 ) ;
#5372 = CARTESIAN_POINT ( 'NONE',  ( 157.4999999999998579, 178.6200623761337738, -45.00000000000000000 ) ) ;
#5373 = EDGE_LOOP ( 'NONE', ( #15599, #3528, #9688, #28153 ) ) ;
#5374 = DIRECTION ( 'NONE',  ( 0.000000000000000000, 0.000000000000000000, 1.000000000000000000 ) ) ;
#5375 = CARTESIAN_POINT ( 'NONE',  ( -68.57415822541635464, 24.64876300893806160, 95.00000000000000000 ) ) ;
#5376 = VERTEX_POINT ( 'NONE', #19462 ) ;
#5377 = AXIS2_PLACEMENT_3D ( 'NONE', #3602, #5484, #20857 ) ;
#5378 = VECTOR ( 'NONE', #15647, 1000.000000000000000 ) ;
#5379 = CARTESIAN_POINT ( 'NONE',  ( -77.65366760726760731, 134.6132604961730124, 15.48745542953684939 ) ) ;
#5380 = CARTESIAN_POINT ( 'NONE',  ( 106.1557582624860601, 248.1951032683517724, 24.28480840886491876 ) ) ;
#5381 = VERTEX_POINT ( 'NONE', #17301 ) ;
#5382 = ORIENTED_EDGE ( 'NONE', *, *, #12688, .F. ) ;
#5383 = DIRECTION ( 'NONE',  ( 0.4528218681369924892, 0.8916010070300079970, -0.000000000000000000 ) ) ;
#5384 = VERTEX_POINT ( 'NONE', #26062 ) ;
#5385 = ORIENTED_EDGE ( 'NONE', *, *, #17804, .T. ) ;
#5386 = ORIENTED_EDGE ( 'NONE', *, *, #1410, .T. ) ;
#5387 = CARTESIAN_POINT ( 'NONE',  ( -212.2419371577844345, -220.0000000000000853, -94.99999999999987210 ) ) ;
#5388 = FACE_OUTER_BOUND ( 'NONE', #12590, .T. ) ;
#5389 = EDGE_CURVE ( 'NONE', #23544, #10546, #19604, .T. ) ;
#5390 = DIRECTION ( 'NONE',  ( 0.8916010070296632728, 0.4528218681376712240, 0.000000000000000000 ) ) ;
#5391 = CIRCLE ( 'NONE', #13678, 30.00000000000000000 ) ;
#5392 = ADVANCED_FACE ( 'NONE', ( #4368 ), #13157, .F. ) ;
#5394 = EDGE_CURVE ( 'NONE', #5589, #15093, #8827, .T. ) ;
#5393 = VECTOR ( 'NONE', #15042, 1000.000000000000000 ) ;
#5395 = CARTESIAN_POINT ( 'NONE',  ( 93.07270601803662657, 112.9533406971499971, -74.06249999970600584 ) ) ;
#5396 = FACE_OUTER_BOUND ( 'NONE', #16065, .T. ) ;
#5397 = FACE_OUTER_BOUND ( 'NONE', #2126, .T. ) ;
#5398 = EDGE_CURVE ( 'NONE', #15531, #27002, #23493, .T. ) ;
#5399 = DIRECTION ( 'NONE',  ( 0.6782242722910298838, 0.7348549764921669114, 0.000000000000000000 ) ) ;
#5400 = LINE ( 'NONE', #952, #5113 ) ;
#5401 = DIRECTION ( 'NONE',  ( -0.4528218681382693567, 0.8916010070293595158, 0.000000000000000000 ) ) ;
#5402 = DIRECTION ( 'NONE',  ( 0.000000000000000000, 0.000000000000000000, 1.000000000000000000 ) ) ;
#5403 = ORIENTED_EDGE ( 'NONE', *, *, #25753, .F. ) ;
#5404 = LINE ( 'NONE', #12032, #5036 ) ;
#5405 = CARTESIAN_POINT ( 'NONE',  ( 158.0000000000005684, 151.2873747973098659, 45.00000000000000000 ) ) ;
#5406 = CARTESIAN_POINT ( 'NONE',  ( 157.9999999999998579, 221.0000000000000284, -45.00000000000000000 ) ) ;
#5407 = ORIENTED_EDGE ( 'NONE', *, *, #1761, .F. ) ;
#5408 = CIRCLE ( 'NONE', #12320, 5.999999999999991118 ) ;
#5409 = DIRECTION ( 'NONE',  ( -0.8916010070298658885, 0.4528218681372721544, 0.000000000000000000 ) ) ;
#5410 = EDGE_LOOP ( 'NONE', ( #6509, #1412, #22952, #16546 ) ) ;
#5411 = LINE ( 'NONE', #828, #387 ) ;
#5412 = AXIS2_PLACEMENT_3D ( 'NONE', #6491, #22144, #17691 ) ;
#5413 = ORIENTED_EDGE ( 'NONE', *, *, #10060, .T. ) ;
#5414 = ORIENTED_EDGE ( 'NONE', *, *, #26964, .T. ) ;
#5415 = EDGE_LOOP ( 'NONE', ( #7116, #5350, #116, #4064 ) ) ;
#5416 = VERTEX_POINT ( 'NONE', #22473 ) ;
#5417 = CARTESIAN_POINT ( 'NONE',  ( -42.53273978471831640, 130.9733465240572627, 14.93735646117640847 ) ) ;
#5418 = LINE ( 'NONE', #972, #28319 ) ;
#5419 = CARTESIAN_POINT ( 'NONE',  ( 282.4999999999996589, 19.41075299063184900, 80.49671038392669686 ) ) ;
#5420 = ADVANCED_FACE ( 'NONE', ( #22184 ), #13724, .F. ) ;
#5421 = ADVANCED_FACE ( 'NONE', ( #782 ), #26474, .T. ) ;
#5422 = AXIS2_PLACEMENT_3D ( 'NONE', #5131, #27108, #4841 ) ;
#5423 = CARTESIAN_POINT ( 'NONE',  ( 157.4999999999998579, 166.0806873385985796, 45.00000000000000000 ) ) ;
#5424 = DIRECTION ( 'NONE',  ( -0.8660254037844454800, -0.4999999999999881206, 0.000000000000000000 ) ) ;
#5425 = EDGE_CURVE ( 'NONE', #19092, #11112, #24198, .T. ) ;
#5426 = CARTESIAN_POINT ( 'NONE',  ( 157.4999999999998579, 148.5255622860493077, 45.00000000000000000 ) ) ;
#5427 = CARTESIAN_POINT ( 'NONE',  ( -97.84640529597095338, 136.0962391708293353, -13.54842801288088161 ) ) ;
#5428 = EDGE_CURVE ( 'NONE', #21920, #3254, #27018, .T. ) ;
#5429 = CARTESIAN_POINT ( 'NONE',  ( 65.00000000000000000, -150.0000000000000568, 64.00000000000002842 ) ) ;
#5430 = VECTOR ( 'NONE', #15578, 1000.000000000000114 ) ;
#5431 = CARTESIAN_POINT ( 'NONE',  ( -217.2892621185082760, 109.4029876883478352, 12.99999999999999822 ) ) ;
#5432 = SURFACE_SIDE_STYLE ('',( #7874 ) ) ;
#5433 = CARTESIAN_POINT ( 'NONE',  ( 186.0596930950812293, 94.49506802741289846, 45.00000000000000000 ) ) ;
#5434 = CYLINDRICAL_SURFACE ( 'NONE', #1081, 24.07986109634097005 ) ;
#5435 = EDGE_LOOP ( 'NONE', ( #22782, #8591, #26320, #25041 ) ) ;
#5436 = PLANE ( 'NONE',  #14659 ) ;
#5437 = LINE ( 'NONE', #26991, #17052 ) ;
#5438 = CARTESIAN_POINT ( 'NONE',  ( -189.5231184314567940, 157.6231267382816554, -15.00000000000000000 ) ) ;
#5440 = ORIENTED_EDGE ( 'NONE', *, *, #20755, .F. ) ;
#5439 = ORIENTED_EDGE ( 'NONE', *, *, #22847, .T. ) ;
#5441 = VECTOR ( 'NONE', #9220, 1000.000000000000000 ) ;
#5442 = DIRECTION ( 'NONE',  ( 0.8916010070296733758, -0.4528218681376511845, 0.000000000000000000 ) ) ;
#5443 = ORIENTED_EDGE ( 'NONE', *, *, #14392, .F. ) ;
#5444 = EDGE_LOOP ( 'NONE', ( #7202, #15181, #8500, #25324, #13483, #17674, #19369, #2587, #23358, #460, #9912, #24920, #263, #8980, #25934, #23719, #3070, #8562, #25601, #1040, #13343, #19688, #22529, #27521, #28362, #4701, #14695, #19614, #21863, #18695, #27803, #22872, #25095, #23438, #24915, #9168, #7561, #12434, #15681, #1485, #1530, #22418, #23738, #1389, #22616, #2089, #16211, #20617, #28380, #23974, #9500, #4386, #17629, #509, #20850, #8253, #5870, #341, #12391, #27763, #10263, #16896, #19293, #3035, #27917, #12006, #23575, #16998, #13544, #3917, #13144, #28340 ) ) ;
#5445 = ORIENTED_EDGE ( 'NONE', *, *, #142, .T. ) ;
#5446 = VECTOR ( 'NONE', #14737, 1000.000000000000000 ) ;
#5447 = AXIS2_PLACEMENT_3D ( 'NONE', #604, #20413, #9367 ) ;
#5448 = ORIENTED_EDGE ( 'NONE', *, *, #15059, .F. ) ;
#5449 = EDGE_CURVE ( 'NONE', #20505, #11364, #26922, .T. ) ;
#5450 = ORIENTED_EDGE ( 'NONE', *, *, #25752, .F. ) ;
#5451 = CARTESIAN_POINT ( 'NONE',  ( 157.4999999999997726, 248.8405625863305204, -45.00000000000000000 ) ) ;
#5452 = LINE ( 'NONE', #14650, #23726 ) ;
#5453 = VECTOR ( 'NONE', #24288, 1000.000000000000000 ) ;
#5454 = ADVANCED_FACE ( 'NONE', ( #22622 ), #11280, .F. ) ;
#5455 = LINE ( 'NONE', #12230, #6399 ) ;
#5456 = CARTESIAN_POINT ( 'NONE',  ( 96.79691392614289214, 232.6553747178996332, -20.12435212500413684 ) ) ;
#5457 = LINE ( 'NONE', #12234, #3207 ) ;
#5458 = AXIS2_PLACEMENT_3D ( 'NONE', #19431, #17271, #4193 ) ;
#5459 = VECTOR ( 'NONE', #15975, 1000.000000000000000 ) ;
#5460 = CARTESIAN_POINT ( 'NONE',  ( 158.0000000000007390, 133.7322497447605656, -45.00000000000000000 ) ) ;
#5461 = FACE_OUTER_BOUND ( 'NONE', #7877, .T. ) ;
#5462 = CARTESIAN_POINT ( 'NONE',  ( -215.1670473708328473, 71.77859382844975755, -26.43926314730827443 ) ) ;
#5463 = AXIS2_PLACEMENT_3D ( 'NONE', #21837, #10631, #2001 ) ;
#5464 = EDGE_CURVE ( 'NONE', #16435, #4097, #2236, .T. ) ;
#5465 = CARTESIAN_POINT ( 'NONE',  ( 112.5180643521146635, 200.1362485301921481, -145.7833319456713639 ) ) ;
#5466 = DIRECTION ( 'NONE',  ( -0.000000000000000000, -0.000000000000000000, -1.000000000000000000 ) ) ;
#5467 = FACE_OUTER_BOUND ( 'NONE', #16177, .T. ) ;
#5468 = DIRECTION ( 'NONE',  ( 0.9961946980917455452, 1.067350013832299517E-17, 0.08715574274765836016 ) ) ;
#5469 = ORIENTED_EDGE ( 'NONE', *, *, #8870, .F. ) ;
#5470 = CARTESIAN_POINT ( 'NONE',  ( 116.5224093497741364, 227.6536686473013447, 45.00000000000000000 ) ) ;
#5471 = CIRCLE ( 'NONE', #9610, 6.025000000000002132 ) ;
#5472 = CARTESIAN_POINT ( 'NONE',  ( -230.6117145417363190, 64.61843588005640981, 16.59905221104221695 ) ) ;
#5473 = CARTESIAN_POINT ( 'NONE',  ( 158.0000000000000000, 206.4606249624626457, -45.00000000000000000 ) ) ;
#5474 = ORIENTED_EDGE ( 'NONE', *, *, #7241, .F. ) ;
#5475 = DIRECTION ( 'NONE',  ( 0.9810645879923677315, 0.1936808565330234710, 0.000000000000000000 ) ) ;
#5476 = VERTEX_POINT ( 'NONE', #13293 ) ;
#5477 = EDGE_CURVE ( 'NONE', #10903, #10018, #16476, .T. ) ;
#5478 = CARTESIAN_POINT ( 'NONE',  ( 109.9999999999999147, 137.0808454111986237, 89.99999999939370809 ) ) ;
#5479 = VECTOR ( 'NONE', #15850, 1000.000000000000000 ) ;
#5480 = PLANE ( 'NONE',  #27324 ) ;
#5481 = VERTEX_POINT ( 'NONE', #19884 ) ;
#5482 = AXIS2_PLACEMENT_3D ( 'NONE', #18904, #12316, #21058 ) ;
#5483 = ORIENTED_EDGE ( 'NONE', *, *, #7657, .T. ) ;
#5484 = DIRECTION ( 'NONE',  ( 0.000000000000000000, -1.000000000000000000, -0.000000000000000000 ) ) ;
#5485 = CIRCLE ( 'NONE', #16531, 10.00000000000000888 ) ;
#5486 = EDGE_CURVE ( 'NONE', #7588, #27001, #20169, .T. ) ;
#5487 = DIRECTION ( 'NONE',  ( -0.000000000000000000, -0.000000000000000000, -1.000000000000000000 ) ) ;
#5488 = CARTESIAN_POINT ( 'NONE',  ( -210.7172313291012529, 103.7585653882801182, 15.00000000000000000 ) ) ;
#5489 = ORIENTED_EDGE ( 'NONE', *, *, #2154, .F. ) ;
#5490 = CARTESIAN_POINT ( 'NONE',  ( 157.4999999999998579, 171.0964373536126573, -45.00000000000000000 ) ) ;
#5491 = ORIENTED_EDGE ( 'NONE', *, *, #10051, .F. ) ;
#5492 = CARTESIAN_POINT ( 'NONE',  ( 158.0000000000006537, 145.7637497747887210, 45.00000000000000000 ) ) ;
#5493 = AXIS2_PLACEMENT_3D ( 'NONE', #15225, #26399, #15651 ) ;
#5494 = DIRECTION ( 'NONE',  ( -0.8379557447115549840, -0.5457381880580680633, 0.000000000000000000 ) ) ;
#5495 = CARTESIAN_POINT ( 'NONE',  ( 158.0000000000015916, 55.48024950453520177, 45.00000000000000000 ) ) ;
#5496 = DIRECTION ( 'NONE',  ( 0.8916010070293409751, 0.4528218681383056610, 0.000000000000000000 ) ) ;
#5497 = CARTESIAN_POINT ( 'NONE',  ( -175.0000000000000000, -120.0000000000001847, -64.00000000000000000 ) ) ;
#5498 = EDGE_CURVE ( 'NONE', #15391, #15494, #4643, .T. ) ;
#5499 = CARTESIAN_POINT ( 'NONE',  ( -272.4438906011233712, -165.0368527442270477, -87.32790004433633158 ) ) ;
#5500 = CARTESIAN_POINT ( 'NONE',  ( -279.3160071107327553, -91.18033988749907337, 0.000000000000000000 ) ) ;
#5501 = ORIENTED_EDGE ( 'NONE', *, *, #27229, .T. ) ;
#5502 = ADVANCED_FACE ( 'NONE', ( #17728 ), #9258, .F. ) ;
#5503 = VECTOR ( 'NONE', #24364, 1000.000000000000114 ) ;
#5504 = DIRECTION ( 'NONE',  ( -0.6681556583950086781, 0.7440215159219069063, 0.000000000000000000 ) ) ;
#5505 = DIRECTION ( 'NONE',  ( -0.000000000000000000, -0.000000000000000000, -1.000000000000000000 ) ) ;
#5506 = DIRECTION ( 'NONE',  ( 1.000000000000000000, -0.000000000000000000, -0.000000000000000000 ) ) ;
#5507 = ORIENTED_EDGE ( 'NONE', *, *, #1882, .T. ) ;
#5508 = CARTESIAN_POINT ( 'NONE',  ( -66.26041567618258910, 130.4659900502583127, 45.00000000000000000 ) ) ;
#5509 = AXIS2_PLACEMENT_3D ( 'NONE', #14430, #9692, #9832 ) ;
#5510 = ORIENTED_EDGE ( 'NONE', *, *, #10062, .T. ) ;
#5511 = CIRCLE ( 'NONE', #14683, 20.24534822868278994 ) ;
#5512 = CARTESIAN_POINT ( 'NONE',  ( -175.0000000000000000, -120.0250000000001762, 70.00000000000001421 ) ) ;
#5513 = DIRECTION ( 'NONE',  ( 0.8660254037844394848, -0.4999999999999985012, 0.000000000000000000 ) ) ;
#5514 = LINE ( 'NONE', #9693, #4821 ) ;
#5515 = ORIENTED_EDGE ( 'NONE', *, *, #17984, .T. ) ;
#5516 =( LENGTH_UNIT ( ) NAMED_UNIT ( * ) SI_UNIT ( .MILLI., .METRE. ) );
#5517 = DIRECTION ( 'NONE',  ( -0.000000000000000000, -0.000000000000000000, 1.000000000000000000 ) ) ;
#5518 = VERTEX_POINT ( 'NONE', #13579 ) ;
#5519 = ADVANCED_FACE ( 'NONE', ( #24334 ), #13431, .F. ) ;
#5520 = CARTESIAN_POINT ( 'NONE',  ( -180.0000000000000284, -2.775557561562891982E-14, 70.00000000000001421 ) ) ;
#5521 = DIRECTION ( 'NONE',  ( 1.000000000000000000, -0.000000000000000000, -0.000000000000000000 ) ) ;
#5522 = VERTEX_POINT ( 'NONE', #354 ) ;
#5523 = EDGE_CURVE ( 'NONE', #19520, #17350, #11571, .T. ) ;
#5524 = ORIENTED_EDGE ( 'NONE', *, *, #8976, .F. ) ;
#5525 = ADVANCED_FACE ( 'NONE', ( #18170 ), #7247, .F. ) ;
#5526 = CARTESIAN_POINT ( 'NONE',  ( -210.0000000000000568, -210.8114316696540982, -110.0000000000000284 ) ) ;
#5527 = ORIENTED_EDGE ( 'NONE', *, *, #20503, .F. ) ;
#5528 = AXIS2_PLACEMENT_3D ( 'NONE', #17015, #3801, #7834 ) ;
#5529 = ADVANCED_FACE ( 'NONE', ( #13869 ), #12239, .F. ) ;
#5530 = EDGE_LOOP ( 'NONE', ( #11034, #7616, #27944, #16929 ) ) ;
#5531 = ORIENTED_EDGE ( 'NONE', *, *, #14454, .T. ) ;
#5532 = CARTESIAN_POINT ( 'NONE',  ( 109.9999999999999005, 260.0000000000000000, 45.00000000000000000 ) ) ;
#5533 = AXIS2_PLACEMENT_3D ( 'NONE', #4685, #393, #253 ) ;
#5534 = CARTESIAN_POINT ( 'NONE',  ( -210.0000000000000000, -212.3568517473289035, 110.0000000000000000 ) ) ;
#5535 = CARTESIAN_POINT ( 'NONE',  ( 157.4999999999997158, 261.3799376238655441, -45.00000000000000000 ) ) ;
#5536 = LINE ( 'NONE', #4962, #17455 ) ;
#5537 = CARTESIAN_POINT ( 'NONE',  ( -17.24491960465746132, -23.01420295945612082, 95.00000000000000000 ) ) ;
#5538 = LINE ( 'NONE', #16195, #11127 ) ;
#5539 = CARTESIAN_POINT ( 'NONE',  ( 157.4999999999998579, 220.0000000000000284, -105.0000000000000284 ) ) ;
#5540 = EDGE_CURVE ( 'NONE', #21098, #4583, #17873, .T. ) ;
#5541 = CARTESIAN_POINT ( 'NONE',  ( -267.2505360800719814, -170.7220645054522663, 109.5009084174815541 ) ) ;
#5542 = DIRECTION ( 'NONE',  ( 0.2588190451025321748, 0.9659258262890653146, 0.000000000000000000 ) ) ;
#5543 = DIRECTION ( 'NONE',  ( 0.000000000000000000, -1.000000000000000000, 0.000000000000000000 ) ) ;
#5544 = ORIENTED_EDGE ( 'NONE', *, *, #17499, .F. ) ;
#5545 = CARTESIAN_POINT ( 'NONE',  ( -6.707964895605361022, 133.1658889964437549, 15.75304700660547574 ) ) ;
#5546 = CIRCLE ( 'NONE', #18848, 2.000000000000003109 ) ;
#5547 = DIRECTION ( 'NONE',  ( -0.000000000000000000, -0.000000000000000000, -1.000000000000000000 ) ) ;
#5548 = CARTESIAN_POINT ( 'NONE',  ( 29.38151960293523501, 82.99431933797082195, 99.87622392724593112 ) ) ;
#5549 = FILL_AREA_STYLE_COLOUR ( '', #11405 ) ;
#5550 = PLANE ( 'NONE',  #25315 ) ;
#5551 = VERTEX_POINT ( 'NONE', #12797 ) ;
#5552 = VECTOR ( 'NONE', #1717, 1000.000000000000000 ) ;
#5553 = FACE_OUTER_BOUND ( 'NONE', #10103, .T. ) ;
#5554 = VERTEX_POINT ( 'NONE', #21544 ) ;
#5555 = CARTESIAN_POINT ( 'NONE',  ( -279.1278187736259611, -165.0000000000001137, -106.1966075482097978 ) ) ;
#5556 = VERTEX_POINT ( 'NONE', #18308 ) ;
#5557 = ADVANCED_FACE ( 'NONE', ( #10491 ), #18966, .T. ) ;
#5558 = ORIENTED_EDGE ( 'NONE', *, *, #13406, .F. ) ;
#5559 = EDGE_CURVE ( 'NONE', #17744, #5793, #16676, .T. ) ;
#5560 = VERTEX_POINT ( 'NONE', #5751 ) ;
#5561 = ORIENTED_EDGE ( 'NONE', *, *, #11675, .F. ) ;
#5562 = ORIENTED_EDGE ( 'NONE', *, *, #1145, .F. ) ;
#5563 = CYLINDRICAL_SURFACE ( 'NONE', #21882, 6.000000000000032863 ) ;
#5564 = CARTESIAN_POINT ( 'NONE',  ( -290.0000000000001705, -157.0000000000000284, -59.99999999999986500 ) ) ;
#5565 = LINE ( 'NONE', #20513, #10671 ) ;
#5566 = VECTOR ( 'NONE', #26512, 1000.000000000000114 ) ;
#5567 = DIRECTION ( 'NONE',  ( -0.000000000000000000, -0.000000000000000000, -1.000000000000000000 ) ) ;
#5568 =( GEOMETRIC_REPRESENTATION_CONTEXT ( 3 ) GLOBAL_UNCERTAINTY_ASSIGNED_CONTEXT ( ( #9749 ) ) GLOBAL_UNIT_ASSIGNED_CONTEXT ( ( #17558, #26319, #4055 ) ) REPRESENTATION_CONTEXT ( 'NONE', 'WORKASPACE' ) );
#5569 = VECTOR ( 'NONE', #7744, 1000.000000000000000 ) ;
#5570 = CARTESIAN_POINT ( 'NONE',  ( -194.4086842179900714, 63.14614340836796913, 41.97977085781615614 ) ) ;
#5571 = DIRECTION ( 'NONE',  ( -0.4999999999999985012, -0.8660254037844394848, 0.000000000000000000 ) ) ;
#5572 = PLANE ( 'NONE',  #23221 ) ;
#5573 = ADVANCED_FACE ( 'NONE', ( #21259 ), #27710, .T. ) ;
#5574 = DIRECTION ( 'NONE',  ( 0.000000000000000000, 0.000000000000000000, -1.000000000000000000 ) ) ;
#5575 = DIRECTION ( 'NONE',  ( 1.000000000000000000, 0.000000000000000000, -0.000000000000000000 ) ) ;
#5576 = DIRECTION ( 'NONE',  ( -0.000000000000000000, -0.000000000000000000, -1.000000000000000000 ) ) ;
#5577 = DIRECTION ( 'NONE',  ( 0.000000000000000000, 0.000000000000000000, 1.000000000000000000 ) ) ;
#5578 = FACE_OUTER_BOUND ( 'NONE', #11855, .T. ) ;
#5579 = ORIENTED_EDGE ( 'NONE', *, *, #3883, .T. ) ;
#5580 = EDGE_CURVE ( 'NONE', #7774, #962, #14661, .T. ) ;
#5581 = CARTESIAN_POINT ( 'NONE',  ( 157.4999999999998295, 231.2854375337815327, 45.00000000000000000 ) ) ;
#5582 = DIRECTION ( 'NONE',  ( 1.000000000000000000, 0.000000000000000000, 0.000000000000000000 ) ) ;
#5583 = DIRECTION ( 'NONE',  ( -0.9985600561963493549, -0.05364526231778204285, 0.000000000000000000 ) ) ;
#5585 = ORIENTED_EDGE ( 'NONE', *, *, #11957, .T. ) ;
#5584 = EDGE_LOOP ( 'NONE', ( #2684, #22836 ) ) ;
#5586 = AXIS2_PLACEMENT_3D ( 'NONE', #22763, #27198, #9407 ) ;
#5587 = CARTESIAN_POINT ( 'NONE',  ( 232.4999999999996305, 186.4134324495536248, -35.02193266779035952 ) ) ;
#5588 = VERTEX_POINT ( 'NONE', #1580 ) ;
#5589 = VERTEX_POINT ( 'NONE', #19249 ) ;
#5590 = EDGE_CURVE ( 'NONE', #24084, #16325, #27993, .T. ) ;
#5591 = ORIENTED_EDGE ( 'NONE', *, *, #12296, .T. ) ;
#5592 = EDGE_CURVE ( 'NONE', #14086, #6262, #1298, .T. ) ;
#5593 = VECTOR ( 'NONE', #6539, 1000.000000000000000 ) ;
#5594 = EDGE_CURVE ( 'NONE', #10330, #7481, #1434, .T. ) ;
#5595 = ORIENTED_EDGE ( 'NONE', *, *, #20567, .T. ) ;
#5596 = ORIENTED_EDGE ( 'NONE', *, *, #4895, .F. ) ;
#5597 = FACE_OUTER_BOUND ( 'NONE', #28263, .T. ) ;
#5598 = DIRECTION ( 'NONE',  ( 0.000000000000000000, 0.000000000000000000, 1.000000000000000000 ) ) ;
#5599 = CARTESIAN_POINT ( 'NONE',  ( 79.99999999999992895, 230.0000000000000284, 45.00000000000000000 ) ) ;
#5600 = CARTESIAN_POINT ( 'NONE',  ( 109.2201764734642495, 251.9989660840318209, -38.05726333473669598 ) ) ;
#5601 = FACE_BOUND ( 'NONE', #12836, .T. ) ;
#5602 = AXIS2_PLACEMENT_3D ( 'NONE', #20556, #7498, #881 ) ;
#5603 = APPLICATION_CONTEXT ( 'automotive_design' ) ;
#5604 = PLANE ( 'NONE',  #9875 ) ;
#5605 = AXIS2_PLACEMENT_3D ( 'NONE', #19916, #13757, #11161 ) ;
#5606 = FACE_OUTER_BOUND ( 'NONE', #4804, .T. ) ;
#5607 = DIRECTION ( 'NONE',  ( 1.000000000000000000, 0.000000000000000000, 0.000000000000000000 ) ) ;
#5608 = CARTESIAN_POINT ( 'NONE',  ( -214.2335385402416534, 55.09354448559546569, -44.71599978583095236 ) ) ;
#5609 = VECTOR ( 'NONE', #11796, 1000.000000000000000 ) ;
#5610 = CARTESIAN_POINT ( 'NONE',  ( 222.4999999999996021, 0.000000000000000000, 0.000000000000000000 ) ) ;
#5611 = CARTESIAN_POINT ( 'NONE',  ( 158.0000000000013927, 73.54324956459154805, 45.00000000000000000 ) ) ;
#5612 = DIRECTION ( 'NONE',  ( 0.000000000000000000, 0.000000000000000000, -1.000000000000000000 ) ) ;
#5613 = ORIENTED_EDGE ( 'NONE', *, *, #10894, .T. ) ;
#5614 = DIRECTION ( 'NONE',  ( 1.000000000000000000, 0.000000000000000000, 0.000000000000000000 ) ) ;
#5615 = ADVANCED_FACE ( 'NONE', ( #8048 ), #16817, .F. ) ;
#5616 = DIRECTION ( 'NONE',  ( 0.000000000000000000, 0.000000000000000000, 1.000000000000000000 ) ) ;
#5617 = VERTEX_POINT ( 'NONE', #7393 ) ;
#5618 = DIRECTION ( 'NONE',  ( 1.000000000000000000, 0.000000000000000000, 0.000000000000000000 ) ) ;
#5619 = ORIENTED_EDGE ( 'NONE', *, *, #20861, .T. ) ;
#5620 = VECTOR ( 'NONE', #17254, 1000.000000000000000 ) ;
#5621 = VERTEX_POINT ( 'NONE', #16159 ) ;
#5622 = CIRCLE ( 'NONE', #19853, 27.00000000000002487 ) ;
#5623 = DIRECTION ( 'NONE',  ( -0.8916010070295820045, -0.4528218681378310406, 0.000000000000000000 ) ) ;
#5624 = FACE_OUTER_BOUND ( 'NONE', #10300, .T. ) ;
#5625 = EDGE_CURVE ( 'NONE', #20966, #24930, #6366, .T. ) ;
#5626 = ORIENTED_EDGE ( 'NONE', *, *, #20964, .T. ) ;
#5627 = AXIS2_PLACEMENT_3D ( 'NONE', #21043, #25363, #1229 ) ;
#5628 = EDGE_LOOP ( 'NONE', ( #14643, #11590, #24587, #20963 ) ) ;
#5629 = CARTESIAN_POINT ( 'NONE',  ( 157.4999999999998579, 193.6673124211760353, -45.00000000000000000 ) ) ;
#5630 = CIRCLE ( 'NONE', #14831, 6.000000000000005329 ) ;
#5631 = EDGE_CURVE ( 'NONE', #16686, #20219, #12358, .T. ) ;
#5632 = CARTESIAN_POINT ( 'NONE',  ( 98.66162091205576701, 233.9456586972327727, 21.50625937152093670 ) ) ;
#5633 = CARTESIAN_POINT ( 'NONE',  ( 157.9999999999996589, 273.6653751576470768, 45.00000000000000000 ) ) ;
#5634 = ORIENTED_EDGE ( 'NONE', *, *, #799, .T. ) ;
#5635 = LINE ( 'NONE', #3328, #25658 ) ;
#5636 = ORIENTED_EDGE ( 'NONE', *, *, #4631, .T. ) ;
#5637 = VECTOR ( 'NONE', #5076, 1000.000000000000000 ) ;
#5638 = DIRECTION ( 'NONE',  ( -0.000000000000000000, -0.000000000000000000, -1.000000000000000000 ) ) ;
#5639 = DIRECTION ( 'NONE',  ( 0.4528218681374907573, -0.8916010070297548662, 0.000000000000000000 ) ) ;
#5640 = CARTESIAN_POINT ( 'NONE',  ( -49.97791255360778706, 113.2029523930418975, -145.0000000000000000 ) ) ;
#5641 = CARTESIAN_POINT ( 'NONE',  ( 22.58950924271104910, 154.2349915562422780, 15.00000000000000000 ) ) ;
#5642 = CARTESIAN_POINT ( 'NONE',  ( 158.0000000000003979, 168.8424998498591663, 45.00000000000000000 ) ) ;
#5643 = VECTOR ( 'NONE', #12121, 1000.000000000000000 ) ;
#5644 = CARTESIAN_POINT ( 'NONE',  ( 157.4999999999998579, 173.6043123611196961, 45.00000000000000000 ) ) ;
#5645 = CARTESIAN_POINT ( 'NONE',  ( -178.5907483116646119, 110.5436109027794203, -30.33689931536702389 ) ) ;
#5646 = EDGE_LOOP ( 'NONE', ( #1267, #10214, #20044, #20218 ) ) ;
#5647 = AXIS2_PLACEMENT_3D ( 'NONE', #2495, #2210, #11285 ) ;
#5648 = DIRECTION ( 'NONE',  ( 1.000000000000000000, 0.000000000000000000, 0.000000000000000000 ) ) ;
#5649 = CARTESIAN_POINT ( 'NONE',  ( -24.92338318254761020, 127.6681916698425567, -138.9999999999999432 ) ) ;
#5650 = CARTESIAN_POINT ( 'NONE',  ( 157.4999999999998579, 125.9546872184859012, 45.00000000000000000 ) ) ;
#5651 = AXIS2_PLACEMENT_3D ( 'NONE', #986, #3270, #10317 ) ;
#5652 = CARTESIAN_POINT ( 'NONE',  ( 158.0000000000010232, 106.1456246621830957, 45.00000000000000000 ) ) ;
#5653 = ORIENTED_EDGE ( 'NONE', *, *, #14358, .F. ) ;
#5654 = LINE ( 'NONE', #25471, #16046 ) ;
#5655 = VERTEX_POINT ( 'NONE', #5226 ) ;
#5656 = ADVANCED_FACE ( 'NONE', ( #27851, #14012 ), #8188, .F. ) ;
#5657 = LINE ( 'NONE', #23184, #26746 ) ;
#5658 = DIRECTION ( 'NONE',  ( 0.000000000000000000, 0.000000000000000000, -1.000000000000000000 ) ) ;
#5659 = CARTESIAN_POINT ( 'NONE',  ( -210.0000000000000568, 0.000000000000000000, 110.0000000000000284 ) ) ;
#5660 = VERTEX_POINT ( 'NONE', #23562 ) ;
#5661 = CARTESIAN_POINT ( 'NONE',  ( -107.3221550338875687, 69.54464929955099706, 83.00000000000001421 ) ) ;
#5662 = ORIENTED_EDGE ( 'NONE', *, *, #5477, .T. ) ;
#5663 = B_SPLINE_CURVE_WITH_KNOTS ( 'NONE', 3,
 ( #20306, #20591, #3059, #11419, #20164, #640, #914, #9682, #18442, #27194, #7533, #16295, #9823, #5783, #23172, #14558, #3483, #14280, #1610, #14845, #25593, #3338, #23310, #21150, #16983, #21291, #1471, #12270, #21004, #3618, #1332, #14418, #10102, #10380, #23449, #9958, #12410, #25461, #18856, #25737, #19136, #16711 ),
 .UNSPECIFIED., .F., .F.,
 ( 4, 2, 2, 2, 2, 2, 2, 2, 2, 2, 2, 2, 2, 2, 2, 2, 2, 2, 2, 2, 4 ),
 ( 0.01880622955133633145, 0.01998131524074743884, 0.02115640093015854623, 0.02174394377486411900, 0.02233148661956969178, 0.02350657230898078875, 0.02468165799839188920, 0.02585674368780298965, 0.02644428653250852079, 0.02703182937721405193, 0.02820691506662503442, 0.02938200075603601691, 0.03055708644544699593, 0.03173217213485798188, 0.03231971497956351302, 0.03290725782426905111, 0.03408234351368011339, 0.03525742920309117567, 0.03584497204779672763, 0.03643251489250227265, 0.03760760058191342514 ),
 .UNSPECIFIED. ) ;
#5664 = DIRECTION ( 'NONE',  ( -0.000000000000000000, -0.000000000000000000, -1.000000000000000000 ) ) ;
#5665 = LINE ( 'NONE', #18874, #9919 ) ;
#5666 = ORIENTED_EDGE ( 'NONE', *, *, #25685, .F. ) ;
#5667 = VECTOR ( 'NONE', #9069, 1000.000000000000000 ) ;
#5668 = VERTEX_POINT ( 'NONE', #4010 ) ;
#5669 = CARTESIAN_POINT ( 'NONE',  ( -210.0000000000000853, -216.9546086794800601, -109.5971846486504830 ) ) ;
#5670 = EDGE_LOOP ( 'NONE', ( #7050, #22904, #5025 ) ) ;
#5671 = EDGE_CURVE ( 'NONE', #23545, #15321, #3873, .T. ) ;
#5672 = CONICAL_SURFACE ( 'NONE', #3837, 7.475068018844455153, 0.08726646259971666819 ) ;
#5673 = EDGE_CURVE ( 'NONE', #1493, #11930, #4992, .T. ) ;
#5674 = ORIENTED_EDGE ( 'NONE', *, *, #19028, .T. ) ;
#5675 = VERTEX_POINT ( 'NONE', #19390 ) ;
#5676 = VECTOR ( 'NONE', #18447, 1000.000000000000114 ) ;
#5677 = CARTESIAN_POINT ( 'NONE',  ( 109.2808348379980856, 254.3902513976626949, 38.18180188068609482 ) ) ;
#5678 = LINE ( 'NONE', #18886, #14010 ) ;
#5679 = DIRECTION ( 'NONE',  ( 0.000000000000000000, 0.000000000000000000, 1.000000000000000000 ) ) ;
#5680 = ADVANCED_FACE ( 'NONE', ( #13225 ), #26135, .F. ) ;
#5681 = CARTESIAN_POINT ( 'NONE',  ( 116.2340178909016970, 207.5736003696172816, -99.27034901580077531 ) ) ;
#5682 = DIRECTION ( 'NONE',  ( -0.000000000000000000, -0.000000000000000000, -1.000000000000000000 ) ) ;
#5683 = CARTESIAN_POINT ( 'NONE',  ( 2.399999999999999911, 9.411460630883494610E-16, 7.685040811306673270 ) ) ;
#5684 = EDGE_CURVE ( 'NONE', #24273, #19795, #27040, .T. ) ;
#5685 = DIRECTION ( 'NONE',  ( -0.000000000000000000, -0.000000000000000000, -1.000000000000000000 ) ) ;
#5686 = CARTESIAN_POINT ( 'NONE',  ( 158.0000000000006253, 148.2716247822957882, 45.00000000000000000 ) ) ;
#5687 = LINE ( 'NONE', #23213, #11873 ) ;
#5688 = DIRECTION ( 'NONE',  ( -0.000000000000000000, 0.000000000000000000, -1.000000000000000000 ) ) ;
#5689 = ORIENTED_EDGE ( 'NONE', *, *, #78, .F. ) ;
#5690 = AXIS2_PLACEMENT_3D ( 'NONE', #13715, #7238, #634 ) ;
#5691 = CARTESIAN_POINT ( 'NONE',  ( 158.0000000000010800, 101.1298746471690038, 45.00000000000000000 ) ) ;
#5692 = CARTESIAN_POINT ( 'NONE',  ( 107.1321927721269134, 249.6641751418899844, -26.92697050482404819 ) ) ;
#5693 = CARTESIAN_POINT ( 'NONE',  ( 22.72047449844828293, 87.17468966359002991, 99.13026680618094133 ) ) ;
#5694 = ADVANCED_FACE ( 'NONE', ( #2422 ), #15090, .F. ) ;
#5695 = DIRECTION ( 'NONE',  ( 0.000000000000000000, 0.000000000000000000, -1.000000000000000000 ) ) ;
#5696 = CARTESIAN_POINT ( 'NONE',  ( 167.4999999999996589, -5.589247009368157215, 84.99999999999995737 ) ) ;
#5697 = VECTOR ( 'NONE', #16439, 1000.000000000000000 ) ;
#5698 = ORIENTED_EDGE ( 'NONE', *, *, #6331, .F. ) ;
#5699 = DIRECTION ( 'NONE',  ( -0.2383857661250380344, -0.9711705445023436356, 0.000000000000000000 ) ) ;
#5700 = ORIENTED_EDGE ( 'NONE', *, *, #2534, .T. ) ;
#5701 = PLANE ( 'NONE',  #10338 ) ;
#5702 = ORIENTED_EDGE ( 'NONE', *, *, #24700, .T. ) ;
#5703 = ORIENTED_EDGE ( 'NONE', *, *, #11863, .F. ) ;
#5704 = CARTESIAN_POINT ( 'NONE',  ( -92.89132778029807014, 136.4114671995147603, 15.16824819155097259 ) ) ;
#5705 = ORIENTED_EDGE ( 'NONE', *, *, #20182, .T. ) ;
#5706 = ORIENTED_EDGE ( 'NONE', *, *, #14017, .F. ) ;
#5707 = FACE_OUTER_BOUND ( 'NONE', #995, .T. ) ;
#5708 = VECTOR ( 'NONE', #22141, 1000.000000000000000 ) ;
#5709 = CARTESIAN_POINT ( 'NONE',  ( 150.5563491861038870, 236.9705627484768797, -45.00000000000000000 ) ) ;
#5710 = CARTESIAN_POINT ( 'NONE',  ( 39.99999999999995026, -19.99999999999983302, 80.00000000000001421 ) ) ;
#5711 = CARTESIAN_POINT ( 'NONE',  ( 6.071532165918828775E-15, -70.00000000000002842, 100.0000000000000142 ) ) ;
#5712 = CARTESIAN_POINT ( 'NONE',  ( -266.7040755562055097, -170.8232809441065001, -94.50355751542548433 ) ) ;
#5713 = DIRECTION ( 'NONE',  ( 1.000000000000000000, 0.000000000000000000, 0.000000000000000000 ) ) ;
#5714 = CARTESIAN_POINT ( 'NONE',  ( -262.5700334248197123, -171.5995001766305847, 94.99999999990480148 ) ) ;
#5715 = LINE ( 'NONE', #18931, #9461 ) ;
#5716 = LINE ( 'NONE', #1685, #5298 ) ;
#5717 = CARTESIAN_POINT ( 'NONE',  ( -12.24491960465745599, 75.97823757117562593, 80.00000000000001421 ) ) ;
#5718 = LINE ( 'NONE', #3554, #15761 ) ;
#5719 = ORIENTED_EDGE ( 'NONE', *, *, #25282, .T. ) ;
#5720 = EDGE_CURVE ( 'NONE', #19224, #27008, #11458, .T. ) ;
#5721 = DIRECTION ( 'NONE',  ( -0.000000000000000000, -0.000000000000000000, -1.000000000000000000 ) ) ;
#5722 = CARTESIAN_POINT ( 'NONE',  ( 85.37729192593057803, 80.27798593821322015, -100.0000000000000142 ) ) ;
#5724 = VERTEX_POINT ( 'NONE', #8478 ) ;
#5723 = ORIENTED_EDGE ( 'NONE', *, *, #19780, .F. ) ;
#5725 = AXIS2_PLACEMENT_3D ( 'NONE', #22575, #20269, #27015 ) ;
#5726 = CARTESIAN_POINT ( 'NONE',  ( -76.25760768171835480, 221.6666220619077876, 12.99999999999999822 ) ) ;
#5727 = ORIENTED_EDGE ( 'NONE', *, *, #12293, .F. ) ;
#5728 = ORIENTED_EDGE ( 'NONE', *, *, #27879, .T. ) ;
#5729 = VECTOR ( 'NONE', #23323, 1000.000000000000000 ) ;
#5730 = ORIENTED_EDGE ( 'NONE', *, *, #25693, .F. ) ;
#5731 = EDGE_LOOP ( 'NONE', ( #19825, #19189, #11761, #12156 ) ) ;
#5732 = ORIENTED_EDGE ( 'NONE', *, *, #18471, .T. ) ;
#5733 = ORIENTED_EDGE ( 'NONE', *, *, #20344, .F. ) ;
#5734 = LINE ( 'NONE', #9779, #15956 ) ;
#5735 = EDGE_CURVE ( 'NONE', #14118, #8411, #282, .T. ) ;
#5736 = FACE_OUTER_BOUND ( 'NONE', #17102, .T. ) ;
#5737 = AXIS2_PLACEMENT_3D ( 'NONE', #28368, #26368, #19766 ) ;
#5738 = VECTOR ( 'NONE', #14917, 999.9999999999998863 ) ;
#5739 = DIRECTION ( 'NONE',  ( -0.000000000000000000, -0.000000000000000000, -1.000000000000000000 ) ) ;
#5740 = FACE_BOUND ( 'NONE', #5234, .T. ) ;
#5741 = CARTESIAN_POINT ( 'NONE',  ( 157.9999999999998579, 219.0000000000000284, 45.00000000000000000 ) ) ;
#5742 = ADVANCED_FACE ( 'NONE', ( #4303 ), #19959, .F. ) ;
#5743 = AXIS2_PLACEMENT_3D ( 'NONE', #10640, #25857, #6316 ) ;
#5744 = B_SPLINE_CURVE_WITH_KNOTS ( 'NONE', 3,
 ( #25641, #21474, #12874, #25782, #1379, #1789 ),
 .UNSPECIFIED., .F., .F.,
 ( 4, 2, 4 ),
 ( 0.002183620363445708690, 0.002481209646569489634, 0.002778798929693271011 ),
 .UNSPECIFIED. ) ;
#5745 = CARTESIAN_POINT ( 'NONE',  ( 217.4999999999996305, 44.41075299063183479, 100.0000000000000142 ) ) ;
#5746 = CARTESIAN_POINT ( 'NONE',  ( -207.5064340660269693, 75.59749780642115979, -45.29313139209890693 ) ) ;
#5747 = ADVANCED_FACE ( 'NONE', ( #140 ), #4154, .F. ) ;
#5748 = EDGE_CURVE ( 'NONE', #22565, #22186, #7330, .T. ) ;
#5749 = DIRECTION ( 'NONE',  ( 0.8916010070295820045, -0.4528218681378310406, 0.000000000000000000 ) ) ;
#5750 = EDGE_CURVE ( 'NONE', #2012, #24201, #25664, .T. ) ;
#5751 = CARTESIAN_POINT ( 'NONE',  ( 130.0130877889309602, 242.4751130497508029, -45.00000000000000000 ) ) ;
#5752 = DIRECTION ( 'NONE',  ( 0.000000000000000000, 0.000000000000000000, 1.000000000000000000 ) ) ;
#5753 = CARTESIAN_POINT ( 'NONE',  ( 157.9999999999998579, 221.5078750075070104, 45.00000000000000000 ) ) ;
#5754 = EDGE_LOOP ( 'NONE', ( #17741, #15602, #4280, #18138 ) ) ;
#5755 = CARTESIAN_POINT ( 'NONE',  ( -189.5697394631524730, 103.4865528990713841, 32.83955206258175252 ) ) ;
#5756 = DIRECTION ( 'NONE',  ( 0.9659258262890670910, 0.2588190451025251804, 0.000000000000000000 ) ) ;
#5757 = ORIENTED_EDGE ( 'NONE', *, *, #26622, .T. ) ;
#5758 = AXIS2_PLACEMENT_3D ( 'NONE', #27188, #4781, #13566 ) ;
#5759 = VERTEX_POINT ( 'NONE', #4439 ) ;
#5760 = AXIS2_PLACEMENT_3D ( 'NONE', #27501, #7978, #21042 ) ;
#5761 = CIRCLE ( 'NONE', #22754, 5.999999999999977796 ) ;
#5762 = VERTEX_POINT ( 'NONE', #8906 ) ;
#5763 = CARTESIAN_POINT ( 'NONE',  ( 98.15430812625453427, 116.0637945822804795, 100.0000000000432863 ) ) ;
#5764 = DIRECTION ( 'NONE',  ( 1.000000000000000000, 0.000000000000000000, 0.000000000000000000 ) ) ;
#5765 = ORIENTED_EDGE ( 'NONE', *, *, #25375, .T. ) ;
#5766 = VECTOR ( 'NONE', #9184, 1000.000000000000000 ) ;
#5767 = ORIENTED_EDGE ( 'NONE', *, *, #6544, .F. ) ;
#5768 = CARTESIAN_POINT ( 'NONE',  ( 158.0000000000015916, 53.48024950453520177, -45.00000000000000000 ) ) ;
#5769 = LINE ( 'NONE', #10231, #12506 ) ;
#5770 = CYLINDRICAL_SURFACE ( 'NONE', #18769, 43.76444293738735070 ) ;
#5771 = EDGE_LOOP ( 'NONE', ( #20927, #17595, #28024, #26444 ) ) ;
#5772 = CARTESIAN_POINT ( 'NONE',  ( 114.5273445118512967, 107.2595481030940476, 100.0000000000000142 ) ) ;
#5773 = EDGE_LOOP ( 'NONE', ( #3382, #11862, #24319, #7244 ) ) ;
#5774 = DIRECTION ( 'NONE',  ( -0.8916010070293515222, -0.4528218681382848443, 0.000000000000000000 ) ) ;
#5775 = ADVANCED_FACE ( 'NONE', ( #10778 ), #23374, .T. ) ;
#5776 = EDGE_CURVE ( 'NONE', #10648, #13244, #6885, .T. ) ;
#5777 = LINE ( 'NONE', #16563, #19054 ) ;
#5778 = FACE_OUTER_BOUND ( 'NONE', #7198, .T. ) ;
#5779 = FACE_OUTER_BOUND ( 'NONE', #4908, .T. ) ;
#5780 = DIRECTION ( 'NONE',  ( -0.8916010070293584056, 0.4528218681382713551, 0.000000000000000000 ) ) ;
#5781 = VECTOR ( 'NONE', #25160, 1000.000000000000000 ) ;
#5782 = CARTESIAN_POINT ( 'NONE',  ( 158.0000000000014211, 71.03537455708449500, 45.00000000000000000 ) ) ;
#5783 = CARTESIAN_POINT ( 'NONE',  ( 163.1896802570002478, 209.7340148635404944, -141.9885977063035227 ) ) ;
#5784 = EDGE_LOOP ( 'NONE', ( #24640, #24280, #7820 ) ) ;
#5785 = CARTESIAN_POINT ( 'NONE',  ( 167.4999999999996589, 258.6181251126050711, 1.387778780781445676E-14 ) ) ;
#5786 = EDGE_CURVE ( 'NONE', #14926, #5668, #17372, .T. ) ;
#5788 = DIRECTION ( 'NONE',  ( -1.000000000000000000, 0.000000000000000000, 0.000000000000000000 ) ) ;
#5787 = VECTOR ( 'NONE', #18894, 999.9999999999998863 ) ;
#5789 = FACE_OUTER_BOUND ( 'NONE', #19993, .T. ) ;
#5790 = LINE ( 'NONE', #17269, #12127 ) ;
#5791 = ORIENTED_EDGE ( 'NONE', *, *, #28135, .T. ) ;
#5792 = LINE ( 'NONE', #25331, #18314 ) ;
#5793 = VERTEX_POINT ( 'NONE', #573 ) ;
#5794 = EDGE_CURVE ( 'NONE', #23853, #8056, #16375, .T. ) ;
#5795 = CARTESIAN_POINT ( 'NONE',  ( 79.99999999999992895, 230.0000000000000284, 45.00000000000000000 ) ) ;
#5796 = LINE ( 'NONE', #1204, #20196 ) ;
#5797 = CARTESIAN_POINT ( 'NONE',  ( 158.0000000000004832, 161.3188748273380213, 45.00000000000000000 ) ) ;
#5798 = ORIENTED_EDGE ( 'NONE', *, *, #25915, .T. ) ;
#5799 = DIRECTION ( 'NONE',  ( 0.000000000000000000, 0.000000000000000000, 1.000000000000000000 ) ) ;
#5800 = CARTESIAN_POINT ( 'NONE',  ( -76.25760768171835480, 219.6666220619077876, 12.99999999999999822 ) ) ;
#5801 = ORIENTED_EDGE ( 'NONE', *, *, #5312, .F. ) ;
#5802 = LINE ( 'NONE', #8529, #7886 ) ;
#5803 = CARTESIAN_POINT ( 'NONE',  ( 109.9986890988327559, 259.7355369120359683, 44.54193649829915813 ) ) ;
#5804 = ORIENTED_EDGE ( 'NONE', *, *, #9709, .F. ) ;
#5805 = AXIS2_PLACEMENT_3D ( 'NONE', #25205, #12433, #16734 ) ;
#5806 = VERTEX_POINT ( 'NONE', #27132 ) ;
#5807 = CARTESIAN_POINT ( 'NONE',  ( 157.9999999999997158, 263.6338751276190351, 45.00000000000000000 ) ) ;
#5808 = VERTEX_POINT ( 'NONE', #7467 ) ;
#5809 = ORIENTED_EDGE ( 'NONE', *, *, #7517, .F. ) ;
#5810 = ORIENTED_EDGE ( 'NONE', *, *, #7765, .F. ) ;
#5811 = LINE ( 'NONE', #4072, #7501 ) ;
#5812 = EDGE_CURVE ( 'NONE', #5660, #12148, #22832, .T. ) ;
#5813 = DIRECTION ( 'NONE',  ( -1.000000000000000000, -1.321694076934710155E-16, 0.000000000000000000 ) ) ;
#5814 = CARTESIAN_POINT ( 'NONE',  ( -146.6428522700808230, 22.24192588826928585, 83.00000000000001421 ) ) ;
#5815 = CARTESIAN_POINT ( 'NONE',  ( 117.2367070128591422, 206.1781180960884683, -99.61792820886472555 ) ) ;
#5816 = LINE ( 'NONE', #1509, #12206 ) ;
#5817 = CARTESIAN_POINT ( 'NONE',  ( -223.4642351922133230, 61.48957812539607914, -20.50364820523719089 ) ) ;
#5818 = CARTESIAN_POINT ( 'NONE',  ( 0.9552291512637761661, 1.249999999999999556, -7.454565938624108767 ) ) ;
#5819 = PLANE ( 'NONE',  #16588 ) ;
#5820 = CARTESIAN_POINT ( 'NONE',  ( -260.0000000000001137, -165.0000000000001137, -59.99999999999986500 ) ) ;
#5821 = CARTESIAN_POINT ( 'NONE',  ( -310.0000000000001137, -220.0000000000000853, -59.99999999999987210 ) ) ;
#5822 = VECTOR ( 'NONE', #12681, 1000.000000000000114 ) ;
#5823 = ORIENTED_EDGE ( 'NONE', *, *, #8346, .F. ) ;
#5824 = DIRECTION ( 'NONE',  ( -1.000000000000000000, 0.000000000000000000, 0.000000000000000000 ) ) ;
#5825 = VECTOR ( 'NONE', #10163, 1000.000000000000000 ) ;
#5826 = EDGE_CURVE ( 'NONE', #5308, #1670, #7179, .T. ) ;
#5827 = EDGE_CURVE ( 'NONE', #23450, #16902, #15950, .T. ) ;
#5828 = DIRECTION ( 'NONE',  ( -0.000000000000000000, -0.000000000000000000, -1.000000000000000000 ) ) ;
#5829 = CARTESIAN_POINT ( 'NONE',  ( 30.93948709196389402, 81.58894172419465463, 100.0000000000000426 ) ) ;
#5830 = SURFACE_STYLE_FILL_AREA ( #18766 ) ;
#5831 = EDGE_CURVE ( 'NONE', #22969, #10435, #25119, .T. ) ;
#5832 = DIRECTION ( 'NONE',  ( -1.000000000000000000, 0.000000000000000000, 0.000000000000000000 ) ) ;
#5833 = VERTEX_POINT ( 'NONE', #13949 ) ;
#5834 = DIRECTION ( 'NONE',  ( 1.000000000000000000, 0.000000000000000000, 0.000000000000000000 ) ) ;
#5835 = VERTEX_POINT ( 'NONE', #16236 ) ;
#5836 = DIRECTION ( 'NONE',  ( 0.4528218681371322663, 0.8916010070299369428, -0.000000000000000000 ) ) ;
#5837 = ORIENTED_EDGE ( 'NONE', *, *, #18247, .F. ) ;
#5838 = ADVANCED_FACE ( 'NONE', ( #13655 ), #5436, .F. ) ;
#5839 = ORIENTED_EDGE ( 'NONE', *, *, #19351, .T. ) ;
#5840 = CARTESIAN_POINT ( 'NONE',  ( 157.4999999999998295, 218.7460624962465090, 45.00000000000000000 ) ) ;
#5841 = EDGE_CURVE ( 'NONE', #6158, #27297, #14219, .T. ) ;
#5842 = VERTEX_POINT ( 'NONE', #26990 ) ;
#5843 = ORIENTED_EDGE ( 'NONE', *, *, #5625, .T. ) ;
#5844 = CARTESIAN_POINT ( 'NONE',  ( -210.7172313291012529, 103.7585653882801182, -5.000000000000004441 ) ) ;
#5845 = AXIS2_PLACEMENT_3D ( 'NONE', #8175, #23977, #4289 ) ;
#5846 = DIRECTION ( 'NONE',  ( -0.8018642810807398158, -0.5975062131282554700, 0.000000000000000000 ) ) ;
#5847 = CARTESIAN_POINT ( 'NONE',  ( -212.1902656986470390, -220.0000000000000284, -94.18570773969327092 ) ) ;
#5848 = CARTESIAN_POINT ( 'NONE',  ( -79.00187704905532371, 96.44595867864549632, -134.2811822434184137 ) ) ;
#5849 = CARTESIAN_POINT ( 'NONE',  ( -273.6179505379467400, -164.9999999998308624, -86.76301814019983283 ) ) ;
#5850 = DIRECTION ( 'NONE',  ( 1.000000000000000000, 0.000000000000000000, 0.000000000000000000 ) ) ;
#5851 = CARTESIAN_POINT ( 'NONE',  ( 158.0000000000015064, 61.00387452705632541, 45.00000000000000000 ) ) ;
#5852 = CARTESIAN_POINT ( 'NONE',  ( 129.6073710054587309, 249.5117418702950829, -147.6595947404202320 ) ) ;
#5853 = CARTESIAN_POINT ( 'NONE',  ( -229.3359862820369699, 89.05815699785955530, 15.38749228882161368 ) ) ;
#5854 = DIRECTION ( 'NONE',  ( 0.4528218681382910060, 0.8916010070293484135, 0.000000000000000000 ) ) ;
#5855 = CARTESIAN_POINT ( 'NONE',  ( -175.8417606860892874, 246.9430296707336652, -13.00000000000000000 ) ) ;
#5856 = CARTESIAN_POINT ( 'NONE',  ( 158.0000000000013642, 76.05112457209858690, 45.00000000000000000 ) ) ;
#5857 = VERTEX_POINT ( 'NONE', #430 ) ;
#5858 = EDGE_CURVE ( 'NONE', #969, #16733, #22694, .T. ) ;
#5859 = ADVANCED_FACE ( 'NONE', ( #24704 ), #17949, .F. ) ;
#5860 = CARTESIAN_POINT ( 'NONE',  ( 158.0000000000001705, 188.9054999099155054, 45.00000000000000000 ) ) ;
#5861 = CARTESIAN_POINT ( 'NONE',  ( 106.5567364938767838, 210.4612944616921482, -144.2111520032349006 ) ) ;
#5863 = ORIENTED_EDGE ( 'NONE', *, *, #7192, .F. ) ;
#5862 = EDGE_LOOP ( 'NONE', ( #25128, #18581, #23038, #16492 ) ) ;
#5864 = CARTESIAN_POINT ( 'NONE',  ( 98.85598102458322955, 241.6222630368573050, -21.45481330788184238 ) ) ;
#5865 = ORIENTED_EDGE ( 'NONE', *, *, #17352, .T. ) ;
#5866 = ORIENTED_EDGE ( 'NONE', *, *, #17290, .T. ) ;
#5867 = EDGE_CURVE ( 'NONE', #25868, #13840, #13802, .T. ) ;
#5868 = ORIENTED_EDGE ( 'NONE', *, *, #24018, .T. ) ;
#5869 = ORIENTED_EDGE ( 'NONE', *, *, #17328, .F. ) ;
#5870 = ORIENTED_EDGE ( 'NONE', *, *, #22190, .F. ) ;
#5871 = ORIENTED_EDGE ( 'NONE', *, *, #20568, .T. ) ;
#5872 = ADVANCED_FACE ( 'NONE', ( #5158 ), #7770, .T. ) ;
#5873 = LINE ( 'NONE', #25420, #6292 ) ;
#5874 = ADVANCED_FACE ( 'NONE', ( #11790 ), #24985, .F. ) ;
#5875 = B_SPLINE_CURVE_WITH_KNOTS ( 'NONE', 3,
 ( #3950, #1792, #10569, #19325, #15317, #26349, #15028, #23780, #17449, #21621 ),
 .UNSPECIFIED., .F., .F.,
 ( 4, 2, 2, 2, 4 ),
 ( 0.000000000000000000, 0.007751866621267358357, 0.009689833276584160215, 0.01162779993190096207, 0.01550373324253456232 ),
 .UNSPECIFIED. ) ;
#5876 = VECTOR ( 'NONE', #4641, 1000.000000000000000 ) ;
#5877 = CARTESIAN_POINT ( 'NONE',  ( 157.9999999999999432, 211.4763749774776045, 45.00000000000000000 ) ) ;
#5878 = EDGE_CURVE ( 'NONE', #10474, #20004, #13755, .T. ) ;
#5879 = CARTESIAN_POINT ( 'NONE',  ( 109.8784163943440859, 256.7827724119275103, -42.21295053313544088 ) ) ;
#5880 = CARTESIAN_POINT ( 'NONE',  ( -6.888137583864597957, 131.5152179544879800, -16.22191523157399473 ) ) ;
#5881 = DIRECTION ( 'NONE',  ( 0.000000000000000000, 0.000000000000000000, 1.000000000000000000 ) ) ;
#5882 = DIRECTION ( 'NONE',  ( 9.345788444546228164E-17, -0.7071067811865435759, 0.7071067811865514585 ) ) ;
#5883 = CARTESIAN_POINT ( 'NONE',  ( -208.9840953169581894, 74.56930307094893351, -36.91869771329891847 ) ) ;
#5885 = CARTESIAN_POINT ( 'NONE',  ( 47.90501010967909679, 226.8374036014029969, 45.00000000000000000 ) ) ;
#5884 = VECTOR ( 'NONE', #11352, 999.9999999999998863 ) ;
#5886 = DIRECTION ( 'NONE',  ( 0.000000000000000000, 1.000000000000000000, 0.000000000000000000 ) ) ;
#5887 = EDGE_CURVE ( 'NONE', #11179, #3789, #9193, .T. ) ;
#5888 = CARTESIAN_POINT ( 'NONE',  ( 2.399999999999999911, 0.000000000000000000, 0.000000000000000000 ) ) ;
#5889 = DIRECTION ( 'NONE',  ( -1.000000000000000000, 0.000000000000000000, -0.000000000000000000 ) ) ;
#5890 = ORIENTED_EDGE ( 'NONE', *, *, #10649, .T. ) ;
#5891 = LINE ( 'NONE', #5470, #21534 ) ;
#5892 = AXIS2_PLACEMENT_3D ( 'NONE', #4404, #21800, #12908 ) ;
#5893 = CIRCLE ( 'NONE', #7736, 5.000000000000004441 ) ;
#5894 = CARTESIAN_POINT ( 'NONE',  ( -271.9547679543769618, -170.1928761609053993, -103.5145866598865183 ) ) ;
#5895 = ORIENTED_EDGE ( 'NONE', *, *, #11648, .F. ) ;
#5896 =( LENGTH_UNIT ( ) NAMED_UNIT ( * ) SI_UNIT ( .MILLI., .METRE. ) );
#5897 = ORIENTED_EDGE ( 'NONE', *, *, #21978, .T. ) ;
#5899 = ORIENTED_EDGE ( 'NONE', *, *, #2367, .T. ) ;
#5898 = CONICAL_SURFACE ( 'NONE', #7310, 14.64217782292691261, 0.08885387018394190484 ) ;
#5900 = CARTESIAN_POINT ( 'NONE',  ( 157.4999999999998579, 85.82868709837320864, 45.00000000000000000 ) ) ;
#5901 = CARTESIAN_POINT ( 'NONE',  ( 157.4999999999998579, 43.19481197075347723, 45.00000000000000000 ) ) ;
#5902 = EDGE_LOOP ( 'NONE', ( #11688, #4767 ) ) ;
#5903 = ORIENTED_EDGE ( 'NONE', *, *, #2015, .T. ) ;
#5904 = LINE ( 'NONE', #5768, #793 ) ;
#5905 = ADVANCED_FACE ( 'NONE', ( #15814 ), #24558, .F. ) ;
#5906 = CARTESIAN_POINT ( 'NONE',  ( 108.4328498615424508, 248.8771578154930069, 35.32563474708244655 ) ) ;
#5907 = CIRCLE ( 'NONE', #7766, 50.00000000000000000 ) ;
#5908 = EDGE_CURVE ( 'NONE', #22677, #21766, #10320, .T. ) ;
#5909 = CARTESIAN_POINT ( 'NONE',  ( -183.2710533429381883, 107.9500601985746897, -30.83634108471951762 ) ) ;
#5910 = ORIENTED_EDGE ( 'NONE', *, *, #2936, .T. ) ;
#5911 = FACE_OUTER_BOUND ( 'NONE', #4105, .T. ) ;
#5912 = ORIENTED_EDGE ( 'NONE', *, *, #22345, .F. ) ;
#5913 = DIRECTION ( 'NONE',  ( 0.7071067811865474617, 8.659560562354932858E-17, 0.7071067811865474617 ) ) ;
#5914 = CIRCLE ( 'NONE', #22432, 100.0000000000000284 ) ;
#5915 = DIRECTION ( 'NONE',  ( -1.000000000000000000, 0.000000000000000000, 0.000000000000000000 ) ) ;
#5916 = DIRECTION ( 'NONE',  ( 0.5804519453834706688, -0.8142945039115421224, 0.000000000000000000 ) ) ;
#5917 = CARTESIAN_POINT ( 'NONE',  ( 134.9999999999998579, 220.0000000000000284, 99.00000000000001421 ) ) ;
#5918 = CARTESIAN_POINT ( 'NONE',  ( -180.0000000000000284, -40.00000000000004974, -70.00000000000001421 ) ) ;
#5919 = CIRCLE ( 'NONE', #16520, 35.18636678425504982 ) ;
#5920 = AXIS2_PLACEMENT_3D ( 'NONE', #2299, #8923, #15973 ) ;
#5921 = DIRECTION ( 'NONE',  ( -0.000000000000000000, -1.000000000000000000, -0.000000000000000000 ) ) ;
#5922 = CARTESIAN_POINT ( 'NONE',  ( -196.6548244826268785, 98.17949491351788538, -32.15600783193318080 ) ) ;
#5923 = ORIENTED_EDGE ( 'NONE', *, *, #2365, .T. ) ;
#5924 = FACE_OUTER_BOUND ( 'NONE', #26826, .T. ) ;
#5925 = CARTESIAN_POINT ( 'NONE',  ( 232.4999999999996305, 83.06687458711267880, 42.88984227207694033 ) ) ;
#5926 = CARTESIAN_POINT ( 'NONE',  ( 157.9999999999997442, 253.6023750975910502, 45.00000000000000000 ) ) ;
#5927 = CARTESIAN_POINT ( 'NONE',  ( 158.0000000000002558, 183.3818748873943889, 45.00000000000000000 ) ) ;
#5928 = ORIENTED_EDGE ( 'NONE', *, *, #21612, .T. ) ;
#5929 = DIRECTION ( 'NONE',  ( -0.000000000000000000, -0.000000000000000000, -1.000000000000000000 ) ) ;
#5930 = EDGE_LOOP ( 'NONE', ( #1167, #21949, #23539, #4306 ) ) ;
#5931 = AXIS2_PLACEMENT_3D ( 'NONE', #7184, #11509, #13807 ) ;
#5932 = CARTESIAN_POINT ( 'NONE',  ( -28.05246235954390244, 188.0718642840173516, -15.00000000000000000 ) ) ;
#5933 = CARTESIAN_POINT ( 'NONE',  ( 157.9999999999996874, 268.6496251426330559, 45.00000000000000000 ) ) ;
#5934 = CARTESIAN_POINT ( 'NONE',  ( -208.4828279284123482, 89.67248562427096203, 24.76657354760775220 ) ) ;
#5935 = ORIENTED_EDGE ( 'NONE', *, *, #22521, .T. ) ;
#5936 = CARTESIAN_POINT ( 'NONE',  ( -295.0000000000002274, -152.0000000000000284, -59.99999999999986500 ) ) ;
#5937 = AXIS2_PLACEMENT_3D ( 'NONE', #20996, #1459, #10234 ) ;
#5938 = DIRECTION ( 'NONE',  ( 0.000000000000000000, -1.000000000000000000, -1.214306433183764966E-16 ) ) ;
#5939 = EDGE_LOOP ( 'NONE', ( #26486, #25208, #27890, #11593 ) ) ;
#5940 = DIRECTION ( 'NONE',  ( 1.000000000000000000, 0.000000000000000000, 0.000000000000000000 ) ) ;
#5941 = DIRECTION ( 'NONE',  ( -0.8916010070294200229, -0.4528218681381501742, 0.000000000000000000 ) ) ;
#5942 = ORIENTED_EDGE ( 'NONE', *, *, #21515, .F. ) ;
#5943 = ORIENTED_EDGE ( 'NONE', *, *, #24148, .F. ) ;
#5944 = VECTOR ( 'NONE', #11048, 1000.000000000000114 ) ;
#5945 = EDGE_CURVE ( 'NONE', #22383, #11368, #6774, .T. ) ;
#5946 = CYLINDRICAL_SURFACE ( 'NONE', #20961, 7.499999999999992895 ) ;
#5947 = ORIENTED_EDGE ( 'NONE', *, *, #5242, .T. ) ;
#5948 = ADVANCED_FACE ( 'NONE', ( #20813 ), #17062, .T. ) ;
#5949 = VERTEX_POINT ( 'NONE', #8308 ) ;
#5950 = ORIENTED_EDGE ( 'NONE', *, *, #27441, .T. ) ;
#5951 = DIRECTION ( 'NONE',  ( -0.8916010070293283185, -0.4528218681383305855, 0.000000000000000000 ) ) ;
#5952 = VECTOR ( 'NONE', #7418, 1000.000000000000000 ) ;
#5953 = DIRECTION ( 'NONE',  ( -2.312964634635743450E-16, 1.000000000000000000, 0.000000000000000000 ) ) ;
#5954 = CARTESIAN_POINT ( 'NONE',  ( -175.0000000000000000, -150.0000000000000853, 64.00000000000002842 ) ) ;
#5955 = CARTESIAN_POINT ( 'NONE',  ( 157.4999999999997726, 243.8248125713165280, -45.00000000000000000 ) ) ;
#5956 = DIRECTION ( 'NONE',  ( 0.8916010070297948342, -0.4528218681374120425, 0.000000000000000000 ) ) ;
#5957 = AXIS2_PLACEMENT_3D ( 'NONE', #19610, #25787, #25928 ) ;
#5958 = DIRECTION ( 'NONE',  ( 0.000000000000000000, 0.000000000000000000, -1.000000000000000000 ) ) ;
#5959 = CARTESIAN_POINT ( 'NONE',  ( 119.9999999999999147, 236.7705098312484893, -100.0000000000000284 ) ) ;
#5960 = VERTEX_POINT ( 'NONE', #16511 ) ;
#5961 = DIRECTION ( 'NONE',  ( 0.000000000000000000, -1.000000000000000000, -1.214306433183764966E-16 ) ) ;
#5962 = CIRCLE ( 'NONE', #925, 30.00000000000001421 ) ;
#5963 = DIRECTION ( 'NONE',  ( 0.000000000000000000, -1.000000000000000000, 0.000000000000000000 ) ) ;
#5964 = CARTESIAN_POINT ( 'NONE',  ( 124.9999999999998579, 220.0000000000000284, -119.9999999999999858 ) ) ;
#5965 = DIRECTION ( 'NONE',  ( -0.7071067811865336949, 0.7071067811865614505, 0.000000000000000000 ) ) ;
#5966 = ORIENTED_EDGE ( 'NONE', *, *, #24671, .T. ) ;
#5967 = DIRECTION ( 'NONE',  ( -0.000000000000000000, -0.000000000000000000, 1.000000000000000000 ) ) ;
#5968 = CARTESIAN_POINT ( 'NONE',  ( 158.0000000000015916, 53.48024950453520177, 45.00000000000000000 ) ) ;
#5969 = DIRECTION ( 'NONE',  ( -2.775557561562887407E-16, -3.668437989309015850E-32, 1.000000000000000000 ) ) ;
#5970 = CARTESIAN_POINT ( 'NONE',  ( -210.0000000000000568, 0.000000000000000000, -110.0000000000000284 ) ) ;
#5971 = ORIENTED_EDGE ( 'NONE', *, *, #20762, .T. ) ;
#5972 = EDGE_CURVE ( 'NONE', #6357, #18214, #20609, .T. ) ;
#5973 = AXIS2_PLACEMENT_3D ( 'NONE', #10413, #14450, #8259 ) ;
#5974 = CARTESIAN_POINT ( 'NONE',  ( -236.2689932932674424, 81.43917303656978390, 15.00000000000000355 ) ) ;
#5975 = ORIENTED_EDGE ( 'NONE', *, *, #3251, .T. ) ;
#5976 = LINE ( 'NONE', #19052, #2538 ) ;
#5977 = EDGE_LOOP ( 'NONE', ( #22241, #22737, #9263, #8482 ) ) ;
#5978 = ORIENTED_EDGE ( 'NONE', *, *, #11674, .T. ) ;
#5979 = CARTESIAN_POINT ( 'NONE',  ( -92.90453691731501351, 136.4113017735256221, 13.49169152925984427 ) ) ;
#5980 = VECTOR ( 'NONE', #1427, 1000.000000000000000 ) ;
#5981 = APPLICATION_CONTEXT ( 'automotive_design' ) ;
#5982 = EDGE_CURVE ( 'NONE', #24757, #12396, #14205, .T. ) ;
#5983 = ORIENTED_EDGE ( 'NONE', *, *, #9657, .T. ) ;
#5984 = VERTEX_POINT ( 'NONE', #19080 ) ;
#5985 = DIRECTION ( 'NONE',  ( 1.000000000000000000, 0.000000000000000000, 0.000000000000000000 ) ) ;
#5986 = LINE ( 'NONE', #17467, #16048 ) ;
#5987 = FACE_OUTER_BOUND ( 'NONE', #1772, .T. ) ;
#5988 = EDGE_CURVE ( 'NONE', #9639, #24350, #14778, .T. ) ;
#5989 = DIRECTION ( 'NONE',  ( -1.000000000000000000, -8.673617379884036705E-17, 0.000000000000000000 ) ) ;
#5990 = CARTESIAN_POINT ( 'NONE',  ( -262.3767685073270286, -171.6469394300385432, -89.94931073348448081 ) ) ;
#5991 = DIRECTION ( 'NONE',  ( -0.000000000000000000, -0.000000000000000000, -1.000000000000000000 ) ) ;
#5992 = CARTESIAN_POINT ( 'NONE',  ( 21.78408758738015294, -47.59365313163254285, 99.02387345699440857 ) ) ;
#5993 = CARTESIAN_POINT ( 'NONE',  ( -220.9594934662428614, 86.32379293724815739, -18.24975661118741499 ) ) ;
#5994 = CIRCLE ( 'NONE', #28, 4.999999999999997335 ) ;
#5995 = FACE_OUTER_BOUND ( 'NONE', #2579, .T. ) ;
#5996 = FACE_OUTER_BOUND ( 'NONE', #12465, .T. ) ;
#5997 = DIRECTION ( 'NONE',  ( 0.4528218681382713551, 0.8916010070293584056, -0.000000000000000000 ) ) ;
#5998 = FACE_OUTER_BOUND ( 'NONE', #2146, .T. ) ;
#5999 = PLANE ( 'NONE',  #10249 ) ;
#6000 = ORIENTED_EDGE ( 'NONE', *, *, #19170, .F. ) ;
#6001 = EDGE_CURVE ( 'NONE', #21738, #15321, #6003, .T. ) ;
#6002 = TOROIDAL_SURFACE ( 'NONE', #16113, 72.21503689626331379, 5.000000000000000000 ) ;
#6003 = LINE ( 'NONE', #10181, #17854 ) ;
#6004 = CARTESIAN_POINT ( 'NONE',  ( 119.9999999999999147, 236.7705098312484893, 100.0000000000000142 ) ) ;
#6005 = DIRECTION ( 'NONE',  ( 1.000000000000000000, 0.000000000000000000, 0.000000000000000000 ) ) ;
#6007 = EDGE_LOOP ( 'NONE', ( #1498, #6749, #25884, #9275 ) ) ;
#6006 = EDGE_LOOP ( 'NONE', ( #17833, #13166, #16765, #17256 ) ) ;
#6008 = EDGE_CURVE ( 'NONE', #25446, #4407, #24276, .T. ) ;
#6009 = CARTESIAN_POINT ( 'NONE',  ( 90.84405255075068908, 240.0000000000000568, -6.597066685413930820 ) ) ;
#6010 = ORIENTED_EDGE ( 'NONE', *, *, #19276, .T. ) ;
#6011 = ORIENTED_EDGE ( 'NONE', *, *, #9459, .F. ) ;
#6012 = ORIENTED_EDGE ( 'NONE', *, *, #16045, .T. ) ;
#6013 = AXIS2_PLACEMENT_3D ( 'NONE', #16982, #567, #12829 ) ;
#6014 = VERTEX_POINT ( 'NONE', #8020 ) ;
#6015 = VERTEX_POINT ( 'NONE', #10462 ) ;
#6016 = ORIENTED_EDGE ( 'NONE', *, *, #17543, .F. ) ;
#6017 = LINE ( 'NONE', #24122, #10444 ) ;
#6018 = VECTOR ( 'NONE', #11651, 1000.000000000000000 ) ;
#6019 = EDGE_CURVE ( 'NONE', #9427, #8629, #27824, .T. ) ;
#6020 = EDGE_CURVE ( 'NONE', #21781, #1313, #12632, .T. ) ;
#6021 = DIRECTION ( 'NONE',  ( 0.000000000000000000, 0.000000000000000000, -1.000000000000000000 ) ) ;
#6022 = DIRECTION ( 'NONE',  ( 0.000000000000000000, -1.000000000000000000, -2.498359269027536814E-16 ) ) ;
#6023 = LINE ( 'NONE', #18542, #23409 ) ;
#6024 = CARTESIAN_POINT ( 'NONE',  ( 222.4999999999996021, 194.4107529906318064, -62.90796922943941638 ) ) ;
#6025 = PLANE ( 'NONE',  #8674 ) ;
#6026 = DIRECTION ( 'NONE',  ( 1.000000000000000000, -1.902611372570518757E-15, 0.000000000000000000 ) ) ;
#6027 = EDGE_CURVE ( 'NONE', #883, #21211, #1129, .T. ) ;
#6028 = VECTOR ( 'NONE', #9860, 1000.000000000000000 ) ;
#6029 = CARTESIAN_POINT ( 'NONE',  ( 112.4397516004750202, 200.2253515377324788, -143.6319245046325364 ) ) ;
#6030 = CARTESIAN_POINT ( 'NONE',  ( 232.4999999999996305, 44.41075299063184190, 75.35061095560295996 ) ) ;
#6031 = DIRECTION ( 'NONE',  ( 0.000000000000000000, -1.000000000000000000, 0.000000000000000000 ) ) ;
#6032 = CARTESIAN_POINT ( 'NONE',  ( -233.2943309833541718, 92.06151970357194614, 15.00000000000000000 ) ) ;
#6033 = VECTOR ( 'NONE', #26754, 1000.000000000000114 ) ;
#6034 = ORIENTED_EDGE ( 'NONE', *, *, #8976, .T. ) ;
#6035 = VECTOR ( 'NONE', #28350, 1000.000000000000000 ) ;
#6036 = CARTESIAN_POINT ( 'NONE',  ( 116.2405502098322501, 232.4361285658575014, -99.27293966533116532 ) ) ;
#6037 = EDGE_CURVE ( 'NONE', #9011, #27217, #14634, .T. ) ;
#6038 = AXIS2_PLACEMENT_3D ( 'NONE', #1100, #13770, #2824 ) ;
#6039 = CARTESIAN_POINT ( 'NONE',  ( -273.2081292221210447, -170.0913695707084514, -108.2505382271841086 ) ) ;
#6040 = ORIENTED_EDGE ( 'NONE', *, *, #12231, .T. ) ;
#6041 = APPLICATION_PROTOCOL_DEFINITION ( 'draft international standard', 'automotive_design', 1998, #8551 ) ;
#6042 = EDGE_CURVE ( 'NONE', #26112, #20676, #12212, .T. ) ;
#6043 = ORIENTED_EDGE ( 'NONE', *, *, #20240, .F. ) ;
#6044 = ORIENTED_EDGE ( 'NONE', *, *, #7185, .F. ) ;
#6045 = CARTESIAN_POINT ( 'NONE',  ( 157.9999999999997158, 259.1260001201120531, 45.00000000000000000 ) ) ;
#6046 = DIRECTION ( 'NONE',  ( 0.4528218681376305343, -0.8916010070296839229, 0.000000000000000000 ) ) ;
#6047 = EDGE_LOOP ( 'NONE', ( #16873, #9356, #10053, #17070 ) ) ;
#6048 = ORIENTED_EDGE ( 'NONE', *, *, #10170, .T. ) ;
#6049 = DIRECTION ( 'NONE',  ( -0.8916010070293383105, -0.4528218681383106015, 0.000000000000000000 ) ) ;
#6050 = AXIS2_PLACEMENT_3D ( 'NONE', #1475, #23178, #14851 ) ;
#6051 = CARTESIAN_POINT ( 'NONE',  ( 105.9596802632211450, 242.8245672004252924, 29.94426634347210125 ) ) ;
#6052 = CARTESIAN_POINT ( 'NONE',  ( -191.3965535058103171, 102.3881842207307358, -32.04908598840737000 ) ) ;
#6053 = EDGE_LOOP ( 'NONE', ( #14402, #26758, #191, #10471 ) ) ;
#6054 = CARTESIAN_POINT ( 'NONE',  ( 232.4749999999995964, 133.0668745871126930, 42.86484227207692044 ) ) ;
#6055 = ORIENTED_EDGE ( 'NONE', *, *, #28335, .F. ) ;
#6056 = VECTOR ( 'NONE', #15141, 1000.000000000000000 ) ;
#6057 = AXIS2_PLACEMENT_3D ( 'NONE', #12246, #27302, #16410 ) ;
#6058 = LINE ( 'NONE', #1463, #6571 ) ;
#6059 = DIRECTION ( 'NONE',  ( -0.2588190451025252359, 0.9659258262890672020, 0.000000000000000000 ) ) ;
#6060 = SPHERICAL_SURFACE ( 'NONE', #12300, 35.18636678425505693 ) ;
#6061 = DIRECTION ( 'NONE',  ( 0.8916010070299267287, -0.4528218681371523058, 0.000000000000000000 ) ) ;
#6062 = CARTESIAN_POINT ( 'NONE',  ( -186.8209274618468498, 105.3754588275796209, -32.54694188853392234 ) ) ;
#6063 = ORIENTED_EDGE ( 'NONE', *, *, #17923, .T. ) ;
#6064 = CARTESIAN_POINT ( 'NONE',  ( 158.0000000000003126, 178.3661248723802828, -45.00000000000000000 ) ) ;
#6065 =( BOUNDED_SURFACE ( )  B_SPLINE_SURFACE ( 3, 2, ( 
 ( #16012, #489, #4783 ),
 ( #910, #25046, #5072 ),
 ( #9250, #5356, #14137 ),
 ( #26914, #9679, #635 ),
 ( #18439, #13862, #20449 ),
 ( #26773, #2480, #4923 ),
 ( #27190, #20302, #9401 ),
 ( #16152, #7529, #773 ),
 ( #26615, #6940, #20014 ),
 ( #18012, #11268, #7092 ),
 ( #16292, #7239, #24765 ),
 ( #15873, #22751, #24904 ),
 ( #15726, #24619, #347 ),
 ( #27050, #22611, #3056 ),
 ( #22465, #13716, #2773 ),
 ( #18158, #2921, #11705 ),
 ( #9540, #13569, #5217 ),
 ( #18300, #14004, #9105 ),
 ( #7384, #17863, #11842 ),
 ( #22320, #11416, #2627 ),
 ( #20587, #20161, #16844 ),
 ( #27321, #11982, #19133 ),
 ( #26128, #27458, #8078 ),
 ( #27599, #7937, #25178 ) ),
 .UNSPECIFIED., .F., .F., .F. ) 
 B_SPLINE_SURFACE_WITH_KNOTS ( ( 4, 2, 2, 2, 2, 2, 2, 2, 2, 2, 2, 4 ),
 ( 3, 3 ),
 ( -3.469446951953614189E-18, 0.006932175204370943401, 0.01386435040874189027, 0.01733043801092736327, 0.02079652561311283801, 0.02772870081748378401, 0.03466087602185473349, 0.03639391982294747085, 0.03812696362404020822, 0.04159305122622568296, 0.04852522643059663243, 0.05545740163496757497 ),
 ( 0.000000000000000000, 1.000000000000000000 ),
 .UNSPECIFIED. ) 
 GEOMETRIC_REPRESENTATION_ITEM ( )  RATIONAL_B_SPLINE_SURFACE ( (
 ( 1.000000000000000000, 0.7071067811865475727, 1.000000000000000000),
 ( 1.000000000000000000, 0.7196205501095098711, 1.000000000000000000),
 ( 1.000000000000000000, 0.7318467739635132752, 1.000000000000000000),
 ( 1.000000000000000000, 0.7550137444392899244, 1.000000000000000000),
 ( 1.000000000000000000, 0.7659551710817132930, 1.000000000000000000),
 ( 1.000000000000000000, 0.7809925864113128613, 1.000000000000000000),
 ( 1.000000000000000000, 0.7857889008458237567, 1.000000000000000000),
 ( 1.000000000000000000, 0.7947914178569325250, 1.000000000000000000),
 ( 1.000000000000000000, 0.7989996273462374177, 1.000000000000000000),
 ( 1.000000000000000000, 0.8107003658405596003, 1.000000000000000000),
 ( 1.000000000000000000, 0.8172691060501307003, 1.000000000000000000),
 ( 1.000000000000000000, 0.8277221977076023585, 1.000000000000000000),
 ( 1.000000000000000000, 0.8316078875901102840, 1.000000000000000000),
 ( 1.000000000000000000, 0.8346398751107367842, 1.000000000000000000),
 ( 1.000000000000000000, 0.8351546698963130400, 1.000000000000000000),
 ( 1.000000000000000000, 0.8359930079802355696, 1.000000000000000000),
 ( 1.000000000000000000, 0.8363177555487408821, 1.000000000000000000),
 ( 1.000000000000000000, 0.8370113090867827843, 1.000000000000000000),
 ( 1.000000000000000000, 0.8370994751787733668, 1.000000000000000000),
 ( 1.000000000000000000, 0.8362601742890978240, 1.000000000000000000),
 ( 1.000000000000000000, 0.8342295125018783786, 1.000000000000000000),
 ( 1.000000000000000000, 0.8273091872078748299, 1.000000000000000000),
 ( 1.000000000000000000, 0.8224188864783793518, 1.000000000000000000),
 ( 1.000000000000000000, 0.8161343730438194166, 1.000000000000000000) ) ) 
 REPRESENTATION_ITEM ( '' )  SURFACE ( )  );
#6066 = LINE ( 'NONE', #6208, #1409 ) ;
#6067 = CARTESIAN_POINT ( 'NONE',  ( 158.0000000000013642, 78.05112457209858690, -45.00000000000000000 ) ) ;
#6068 = ADVANCED_FACE ( 'NONE', ( #9902 ), #1555, .F. ) ;
#6069 = LINE ( 'NONE', #1751, #24519 ) ;
#6070 = VERTEX_POINT ( 'NONE', #3418 ) ;
#6071 = VECTOR ( 'NONE', #4112, 1000.000000000000000 ) ;
#6072 = CARTESIAN_POINT ( 'NONE',  ( 115.9275995189148318, 231.9502961609913143, 99.13875753836930471 ) ) ;
#6073 = EDGE_CURVE ( 'NONE', #11332, #15143, #27400, .T. ) ;
#6074 = VECTOR ( 'NONE', #9515, 1000.000000000000000 ) ;
#6075 = DIRECTION ( 'NONE',  ( 1.000000000000000000, -0.000000000000000000, 0.000000000000000000 ) ) ;
#6076 = CARTESIAN_POINT ( 'NONE',  ( 112.5248869502488134, 224.9869122110685282, 45.00000000000000000 ) ) ;
#6077 = CARTESIAN_POINT ( 'NONE',  ( -295.0000000000001705, -170.0000000000001137, -59.99999999999986500 ) ) ;
#6078 = ORIENTED_EDGE ( 'NONE', *, *, #13080, .T. ) ;
#6079 = FACE_OUTER_BOUND ( 'NONE', #25799, .T. ) ;
#6080 = VECTOR ( 'NONE', #18111, 1000.000000000000000 ) ;
#6081 = ORIENTED_EDGE ( 'NONE', *, *, #12030, .F. ) ;
#6082 = VECTOR ( 'NONE', #296, 1000.000000000000000 ) ;
#6083 = DIRECTION ( 'NONE',  ( -0.8916010070293283185, -0.4528218681383305855, 0.000000000000000000 ) ) ;
#6084 = DIRECTION ( 'NONE',  ( -0.000000000000000000, -0.000000000000000000, -1.000000000000000000 ) ) ;
#6085 = ORIENTED_EDGE ( 'NONE', *, *, #1641, .T. ) ;
#6086 = EDGE_LOOP ( 'NONE', ( #7061, #7339, #23901, #24077 ) ) ;
#6087 = FACE_OUTER_BOUND ( 'NONE', #26011, .T. ) ;
#6088 = VERTEX_POINT ( 'NONE', #16650 ) ;
#6089 = EDGE_LOOP ( 'NONE', ( #25056, #20679, #14609, #14583 ) ) ;
#6090 = EDGE_LOOP ( 'NONE', ( #9132, #21389, #28360, #12567 ) ) ;
#6091 = CARTESIAN_POINT ( 'NONE',  ( 222.4999999999996021, 186.4134324495536248, -35.02193266779035952 ) ) ;
#6092 = VECTOR ( 'NONE', #26703, 1000.000000000000000 ) ;
#6093 = EDGE_CURVE ( 'NONE', #18691, #9161, #18782, .T. ) ;
#6094 = LINE ( 'NONE', #19166, #10794 ) ;
#6095 = CARTESIAN_POINT ( 'NONE',  ( 157.9999999999998010, 236.0472500450420341, 45.00000000000000000 ) ) ;
#6096 = DIRECTION ( 'NONE',  ( 1.000000000000000000, 8.673617379884036705E-17, 0.000000000000000000 ) ) ;
#6097 = AXIS2_PLACEMENT_3D ( 'NONE', #9717, #18343, #27091 ) ;
#6098 = AXIS2_PLACEMENT_3D ( 'NONE', #24675, #13199, #2539 ) ;
#6099 = CARTESIAN_POINT ( 'NONE',  ( 158.0000000000000853, 200.9369999399436892, 45.00000000000000000 ) ) ;
#6100 = DIRECTION ( 'NONE',  ( 1.000000000000000000, 1.850371707708592344E-16, 0.000000000000000000 ) ) ;
#6101 = CARTESIAN_POINT ( 'NONE',  ( -239.6893155506592166, 70.91029463948937916, -5.253362301615601027 ) ) ;
#6102 = ORIENTED_EDGE ( 'NONE', *, *, #5275, .F. ) ;
#6103 = CARTESIAN_POINT ( 'NONE',  ( 158.0000000000003126, 178.3661248723802828, 45.00000000000000000 ) ) ;
#6104 = EDGE_CURVE ( 'NONE', #17036, #6791, #16051, .T. ) ;
#6105 = CARTESIAN_POINT ( 'NONE',  ( -227.8378063125350650, 130.6400894613935293, 12.99999999999999822 ) ) ;
#6106 = DIRECTION ( 'NONE',  ( -1.000000000000000000, 0.000000000000000000, 0.000000000000000000 ) ) ;
#6107 = CARTESIAN_POINT ( 'NONE',  ( -24.33210486176665910, 0.000000000000000000, 100.0000000000000000 ) ) ;
#6108 = ORIENTED_EDGE ( 'NONE', *, *, #13682, .T. ) ;
#6109 = EDGE_CURVE ( 'NONE', #20915, #1874, #21804, .T. ) ;
#6110 = CARTESIAN_POINT ( 'NONE',  ( 0.000000000000000000, 75.97823757117562593, 100.0000000000000000 ) ) ;
#6111 = EDGE_CURVE ( 'NONE', #22406, #23236, #2113, .T. ) ;
#6112 = EDGE_CURVE ( 'NONE', #17545, #7637, #21076, .T. ) ;
#6113 = CARTESIAN_POINT ( 'NONE',  ( 39.99999999999995026, -19.99999999999983302, 110.0000000000000284 ) ) ;
#6114 = DIRECTION ( 'NONE',  ( -1.321694076934710155E-16, 1.000000000000000000, 0.000000000000000000 ) ) ;
#6115 = DIRECTION ( 'NONE',  ( -1.000000000000000000, 4.540956701092242152E-16, 0.000000000000000000 ) ) ;
#6116 = LINE ( 'NONE', #14746, #23778 ) ;
#6117 = CARTESIAN_POINT ( 'NONE',  ( 372.9108539694884144, 44.41075299063183479, 74.80456309157131045 ) ) ;
#6118 = EDGE_LOOP ( 'NONE', ( #7668, #22373, #5910, #21610 ) ) ;
#6119 = VECTOR ( 'NONE', #23840, 1000.000000000000114 ) ;
#6120 = CIRCLE ( 'NONE', #24934, 5.999999999999977796 ) ;
#6121 = CARTESIAN_POINT ( 'NONE',  ( -49.97791255360778706, 113.2029523930418975, -145.0000000000000000 ) ) ;
#6122 = ORIENTED_EDGE ( 'NONE', *, *, #13524, .T. ) ;
#6123 = LINE ( 'NONE', #7853, #20923 ) ;
#6124 = EDGE_LOOP ( 'NONE', ( #8360, #14998 ) ) ;
#6125 = VECTOR ( 'NONE', #9297, 1000.000000000000000 ) ;
#6126 = VERTEX_POINT ( 'NONE', #10604 ) ;
#6127 = CARTESIAN_POINT ( 'NONE',  ( -85.28599540134722190, 134.8026027455211988, 15.45364094122273002 ) ) ;
#6128 = ORIENTED_EDGE ( 'NONE', *, *, #6236, .F. ) ;
#6129 = VERTEX_POINT ( 'NONE', #2388 ) ;
#6130 = DIRECTION ( 'NONE',  ( 0.4528218681377911836, -0.8916010070296023216, 0.000000000000000000 ) ) ;
#6131 = CARTESIAN_POINT ( 'NONE',  ( -90.06590765905433216, 134.7839249153333583, -15.45693337243942267 ) ) ;
#6132 = CARTESIAN_POINT ( 'NONE',  ( -211.4917091876254744, -219.2061850725015120, 92.08741365143876578 ) ) ;
#6133 = CARTESIAN_POINT ( 'NONE',  ( -127.8679930504526538, 131.6610752695499400, -14.66658078038128998 ) ) ;
#6134 = VECTOR ( 'NONE', #8469, 1000.000000000000114 ) ;
#6135 = EDGE_CURVE ( 'NONE', #12640, #6070, #12377, .T. ) ;
#6136 = CARTESIAN_POINT ( 'NONE',  ( -274.7557459110828972, -170.0000000000001137, -86.12025961983449918 ) ) ;
#6137 = EDGE_CURVE ( 'NONE', #11692, #22985, #10890, .T. ) ;
#6138 = CARTESIAN_POINT ( 'NONE',  ( 157.4999999999998579, 60.74993702330277756, -45.00000000000000000 ) ) ;
#6139 = CARTESIAN_POINT ( 'NONE',  ( -222.9992919783725824, 86.62858596284870316, -17.32510164567526800 ) ) ;
#6140 = PRODUCT_DEFINITION_SHAPE ( 'NONE', 'NONE',  #28411 ) ;
#6141 = DIRECTION ( 'NONE',  ( 1.000000000000000000, 0.000000000000000000, 0.000000000000000000 ) ) ;
#6142 = ADVANCED_FACE ( 'NONE', ( #19358 ), #19505, .T. ) ;
#6143 = CARTESIAN_POINT ( 'NONE',  ( -209.3833921019910349, 88.44299030055611865, 25.74621063874961280 ) ) ;
#6144 = VECTOR ( 'NONE', #8410, 1000.000000000000114 ) ;
#6145 = FACE_OUTER_BOUND ( 'NONE', #19193, .T. ) ;
#6146 = DIRECTION ( 'NONE',  ( 1.000000000000000000, 0.000000000000000000, 0.000000000000000000 ) ) ;
#6147 = CARTESIAN_POINT ( 'NONE',  ( 157.4999999999998579, 115.9231871884577174, 45.00000000000000000 ) ) ;
#6148 = ORIENTED_EDGE ( 'NONE', *, *, #17431, .F. ) ;
#6149 = EDGE_CURVE ( 'NONE', #28035, #15436, #10363, .T. ) ;
#6150 = CARTESIAN_POINT ( 'NONE',  ( 157.9999999999999147, 215.9842499849850697, 45.00000000000000000 ) ) ;
#6151 = CARTESIAN_POINT ( 'NONE',  ( -143.6428522700808230, 71.54464929955099706, 83.00000000000001421 ) ) ;
#6152 = DIRECTION ( 'NONE',  ( 0.8916010070298658885, -0.4528218681372722099, 0.000000000000000000 ) ) ;
#6154 = ORIENTED_EDGE ( 'NONE', *, *, #23496, .T. ) ;
#6153 = ORIENTED_EDGE ( 'NONE', *, *, #28236, .F. ) ;
#6155 = ADVANCED_FACE ( 'NONE', ( #254 ), #17343, .T. ) ;
#6156 = CARTESIAN_POINT ( 'NONE',  ( 96.93828241644565935, 232.7455409703808016, -20.22303902613517579 ) ) ;
#6157 = ORIENTED_EDGE ( 'NONE', *, *, #5720, .F. ) ;
#6158 = VERTEX_POINT ( 'NONE', #15352 ) ;
#6159 = AXIS2_PLACEMENT_3D ( 'NONE', #16363, #15940, #11916 ) ;
#6160 = ORIENTED_EDGE ( 'NONE', *, *, #13080, .F. ) ;
#6161 = ORIENTED_EDGE ( 'NONE', *, *, #5673, .T. ) ;
#6162 = AXIS2_PLACEMENT_3D ( 'NONE', #27296, #3847, #9516 ) ;
#6163 = ORIENTED_EDGE ( 'NONE', *, *, #25003, .T. ) ;
#6164 = ORIENTED_EDGE ( 'NONE', *, *, #10246, .F. ) ;
#6165 = CARTESIAN_POINT ( 'NONE',  ( 179.9999999999999147, 330.0000000000000000, 84.99999999999995737 ) ) ;
#6166 = DIRECTION ( 'NONE',  ( 1.000000000000000000, -0.000000000000000000, -0.000000000000000000 ) ) ;
#6167 = DIRECTION ( 'NONE',  ( 1.000000000000000000, -0.000000000000000000, -0.000000000000000000 ) ) ;
#6168 = LINE ( 'NONE', #8753, #8751 ) ;
#6169 = ADVANCED_FACE ( 'NONE', ( #8452 ), #13317, .T. ) ;
#6170 = DIRECTION ( 'NONE',  ( 0.000000000000000000, -1.000000000000000000, 0.000000000000000000 ) ) ;
#6171 = CARTESIAN_POINT ( 'NONE',  ( 158.0000000000001137, 193.9212499249295831, 45.00000000000000000 ) ) ;
#6172 = CARTESIAN_POINT ( 'NONE',  ( -225.9870166515752601, 72.66138222772276833, -17.86717049014344383 ) ) ;
#6173 = CIRCLE ( 'NONE', #22699, 35.18636678425505693 ) ;
#6174 = CARTESIAN_POINT ( 'NONE',  ( -40.35410369946821163, 130.4208408520967168, 15.14572397854045249 ) ) ;
#6175 = DIRECTION ( 'NONE',  ( 1.000000000000000000, 0.000000000000000000, -2.775557561562887407E-16 ) ) ;
#6176 = CARTESIAN_POINT ( 'NONE',  ( 158.0000000000005400, 156.3031248123239436, -45.00000000000000000 ) ) ;
#6177 = PLANE ( 'NONE',  #6974 ) ;
#6178 = CIRCLE ( 'NONE', #15365, 9.999999999999996447 ) ;
#6179 = ORIENTED_EDGE ( 'NONE', *, *, #885, .T. ) ;
#6180 = CARTESIAN_POINT ( 'NONE',  ( -178.0751036719780132, 111.1757337266472518, 28.96268686395388059 ) ) ;
#6181 = EDGE_CURVE ( 'NONE', #21202, #23711, #4126, .T. ) ;
#6182 = ADVANCED_FACE ( 'NONE', ( #21941 ), #3982, .F. ) ;
#6183 = DIRECTION ( 'NONE',  ( 0.000000000000000000, 0.000000000000000000, 1.000000000000000000 ) ) ;
#6184 = ORIENTED_EDGE ( 'NONE', *, *, #14358, .T. ) ;
#6185 = SHAPE_DEFINITION_REPRESENTATION ( #21034, #201 ) ;
#6186 = VERTEX_POINT ( 'NONE', #23677 ) ;
#6187 = ORIENTED_EDGE ( 'NONE', *, *, #9397, .F. ) ;
#6188 = CARTESIAN_POINT ( 'NONE',  ( 79.99999999999991473, 110.0000000000000142, 100.0000000000000142 ) ) ;
#6189 = CARTESIAN_POINT ( 'NONE',  ( 79.99999999999995737, 59.99999999999998579, 15.00000000000000000 ) ) ;
#6190 = ORIENTED_EDGE ( 'NONE', *, *, #14879, .F. ) ;
#6191 = VECTOR ( 'NONE', #14804, 1000.000000000000000 ) ;
#6193 = EDGE_CURVE ( 'NONE', #7297, #2370, #6430, .T. ) ;
#6192 = ORIENTED_EDGE ( 'NONE', *, *, #5498, .F. ) ;
#6194 = CARTESIAN_POINT ( 'NONE',  ( 96.92716526686170653, 115.1868982021059935, -100.0000000000216716 ) ) ;
#6195 = EDGE_CURVE ( 'NONE', #24666, #16446, #6708, .T. ) ;
#6196 = CARTESIAN_POINT ( 'NONE',  ( 99.70645294041088391, 234.7926843489850057, 22.37568098243790971 ) ) ;
#6197 = LINE ( 'NONE', #4032, #19219 ) ;
#6198 = ORIENTED_EDGE ( 'NONE', *, *, #5299, .F. ) ;
#6199 = CARTESIAN_POINT ( 'NONE',  ( -207.3017215893796106, 90.23546665973240977, 26.80608177402522685 ) ) ;
#6200 = ORIENTED_EDGE ( 'NONE', *, *, #2124, .F. ) ;
#6201 = CYLINDRICAL_SURFACE ( 'NONE', #18970, 5.999999999999991118 ) ;
#6202 = FACE_OUTER_BOUND ( 'NONE', #215, .T. ) ;
#6203 = CARTESIAN_POINT ( 'NONE',  ( 158.0000000000010800, 103.1298746471690038, -45.00000000000000000 ) ) ;
#6204 = LINE ( 'NONE', #9481, #25732 ) ;
#6205 = ORIENTED_EDGE ( 'NONE', *, *, #17321, .T. ) ;
#6206 = FACE_OUTER_BOUND ( 'NONE', #7500, .T. ) ;
#6207 = CIRCLE ( 'NONE', #26869, 5.999999999999977796 ) ;
#6208 = CARTESIAN_POINT ( 'NONE',  ( -412.2374841615667833, -120.0000000000002558, 100.0000000000000142 ) ) ;
#6209 = DIRECTION ( 'NONE',  ( 0.8916010070294605461, 0.4528218681380702382, 0.000000000000000000 ) ) ;
#6210 = LINE ( 'NONE', #19005, #8915 ) ;
#6211 = ORIENTED_EDGE ( 'NONE', *, *, #10135, .T. ) ;
#6212 = AXIS2_PLACEMENT_3D ( 'NONE', #23362, #21203, #12183 ) ;
#6213 = CARTESIAN_POINT ( 'NONE',  ( 119.9999999999999147, 236.7705098312484893, 100.0000000000000142 ) ) ;
#6214 = ADVANCED_FACE ( 'NONE', ( #6283 ), #22664, .F. ) ;
#6215 = CARTESIAN_POINT ( 'NONE',  ( 157.4999999999998579, 198.6830624361901414, 45.00000000000000000 ) ) ;
#6216 = LINE ( 'NONE', #6076, #9190 ) ;
#6217 = DIRECTION ( 'NONE',  ( -0.000000000000000000, -0.000000000000000000, -1.000000000000000000 ) ) ;
#6218 = ORIENTED_EDGE ( 'NONE', *, *, #23204, .F. ) ;
#6219 = DIRECTION ( 'NONE',  ( 1.000000000000000000, 0.000000000000000000, -0.000000000000000000 ) ) ;
#6220 = AXIS2_PLACEMENT_3D ( 'NONE', #27300, #7912, #22865 ) ;
#6221 = ORIENTED_EDGE ( 'NONE', *, *, #24606, .T. ) ;
#6222 = DIRECTION ( 'NONE',  ( 0.8916010070293584056, -0.4528218681382712996, 0.000000000000000000 ) ) ;
#6223 = CARTESIAN_POINT ( 'NONE',  ( -185.4353359813156601, 106.5295224582049372, -31.86382914232619257 ) ) ;
#6224 = ORIENTED_EDGE ( 'NONE', *, *, #23270, .F. ) ;
#6225 = VERTEX_POINT ( 'NONE', #9451 ) ;
#6226 = DIRECTION ( 'NONE',  ( 0.4528218681383106015, 0.8916010070293384215, -0.000000000000000000 ) ) ;
#6227 = VERTEX_POINT ( 'NONE', #11321 ) ;
#6228 = VECTOR ( 'NONE', #24130, 1000.000000000000000 ) ;
#6229 = ORIENTED_EDGE ( 'NONE', *, *, #14714, .F. ) ;
#6230 = VERTEX_POINT ( 'NONE', #9158 ) ;
#6232 = ADVANCED_FACE ( 'NONE', ( #4832 ), #24669, .F. ) ;
#6231 = VECTOR ( 'NONE', #2757, 1000.000000000000000 ) ;
#6233 = DIRECTION ( 'NONE',  ( 0.000000000000000000, -1.000000000000000000, 0.000000000000000000 ) ) ;
#6234 = ADVANCED_FACE ( 'NONE', ( #7142 ), #22370, .F. ) ;
#6235 = LINE ( 'NONE', #26192, #7144 ) ;
#6236 = EDGE_CURVE ( 'NONE', #14636, #23094, #2681, .T. ) ;
#6237 = SPHERICAL_SURFACE ( 'NONE', #20822, 30.00000000000000000 ) ;
#6238 = SPHERICAL_SURFACE ( 'NONE', #28229, 35.18636678425505693 ) ;
#6239 = VECTOR ( 'NONE', #12407, 1000.000000000000000 ) ;
#6240 = DIRECTION ( 'NONE',  ( 1.000000000000000000, 0.000000000000000000, 0.000000000000000000 ) ) ;
#6241 = FACE_OUTER_BOUND ( 'NONE', #2915, .T. ) ;
#6242 = CARTESIAN_POINT ( 'NONE',  ( -233.5270925705994500, 66.28764270639172196, -15.64035431904813045 ) ) ;
#6243 = EDGE_LOOP ( 'NONE', ( #22004, #1803, #17882, #28030 ) ) ;
#6244 = CARTESIAN_POINT ( 'NONE',  ( 0.000000000000000000, -1.249999999999998890, -8.000000000000000000 ) ) ;
#6245 = DIRECTION ( 'NONE',  ( -0.000000000000000000, -0.000000000000000000, -1.000000000000000000 ) ) ;
#6246 = DIRECTION ( 'NONE',  ( -0.000000000000000000, -0.000000000000000000, 1.000000000000000000 ) ) ;
#6247 = DIRECTION ( 'NONE',  ( 0.000000000000000000, -1.000000000000000000, 0.000000000000000000 ) ) ;
#6248 = EDGE_LOOP ( 'NONE', ( #15713, #24751, #6320, #2348 ) ) ;
#6249 = DIRECTION ( 'NONE',  ( -0.05364526231780537141, -0.9985600561963481336, 0.000000000000000000 ) ) ;
#6250 = CARTESIAN_POINT ( 'NONE',  ( 157.4999999999998579, 156.0491873085704242, 45.00000000000000000 ) ) ;
#6251 = LINE ( 'NONE', #6536, #8241 ) ;
#6252 = CARTESIAN_POINT ( 'NONE',  ( -12.24491960465745599, 75.97823757117562593, 95.00000000000000000 ) ) ;
#6253 = LINE ( 'NONE', #8981, #21626 ) ;
#6254 = LINE ( 'NONE', #27652, #18901 ) ;
#6255 = ORIENTED_EDGE ( 'NONE', *, *, #12010, .T. ) ;
#6256 = AXIS2_PLACEMENT_3D ( 'NONE', #17110, #26150, #4024 ) ;
#6257 = CARTESIAN_POINT ( 'NONE',  ( 157.9999999999997726, 243.5708750675630370, -45.00000000000000000 ) ) ;
#6258 = ORIENTED_EDGE ( 'NONE', *, *, #28312, .T. ) ;
#6259 = CARTESIAN_POINT ( 'NONE',  ( 157.9999999999998010, 239.0630000600560550, 45.00000000000000000 ) ) ;
#6260 = EDGE_LOOP ( 'NONE', ( #25691, #3432, #13702, #25861 ) ) ;
#6261 = AXIS2_PLACEMENT_3D ( 'NONE', #4226, #23916, #26621 ) ;
#6262 = VERTEX_POINT ( 'NONE', #7291 ) ;
#6263 = CARTESIAN_POINT ( 'NONE',  ( -81.50071837300136224, 134.7411680033590358, 15.46448801347469981 ) ) ;
#6264 = EDGE_LOOP ( 'NONE', ( #13399, #26499, #9027, #5719 ) ) ;
#6265 = EDGE_CURVE ( 'NONE', #7514, #6925, #27500, .T. ) ;
#6266 = ORIENTED_EDGE ( 'NONE', *, *, #17104, .F. ) ;
#6267 = CARTESIAN_POINT ( 'NONE',  ( 109.9999999999999147, 140.0000000000000000, -45.00000000000000000 ) ) ;
#6268 = CARTESIAN_POINT ( 'NONE',  ( 199.9999999999997726, -280.0000000000000000, -110.0000000000000284 ) ) ;
#6269 = CARTESIAN_POINT ( 'NONE',  ( 157.4999999999998579, 196.1751874286831026, -45.00000000000000000 ) ) ;
#6270 = EDGE_CURVE ( 'NONE', #7659, #12559, #25686, .T. ) ;
#6271 = EDGE_CURVE ( 'NONE', #16518, #3496, #24377, .T. ) ;
#6272 = CARTESIAN_POINT ( 'NONE',  ( -108.0095164744623730, 135.2230479792049493, -13.71926593627200397 ) ) ;
#6273 = CARTESIAN_POINT ( 'NONE',  ( -141.6428522700808230, 74.54464929955099706, 83.00000000000001421 ) ) ;
#6274 = VECTOR ( 'NONE', #13995, 1000.000000000000000 ) ;
#6275 = LINE ( 'NONE', #16777, #11030 ) ;
#6276 = CARTESIAN_POINT ( 'NONE',  ( -262.5332230410764396, -166.4061304486595532, 89.91977158827830863 ) ) ;
#6277 = CARTESIAN_POINT ( 'NONE',  ( -229.7952689998928690, 91.77895247750312535, -15.17557543154750910 ) ) ;
#6278 = CARTESIAN_POINT ( 'NONE',  ( 130.6168512560825832, 249.6783991519806705, -149.1019530262190358 ) ) ;
#6279 = DIRECTION ( 'NONE',  ( -0.000000000000000000, -0.000000000000000000, -1.000000000000000000 ) ) ;
#6280 = CARTESIAN_POINT ( 'NONE',  ( 367.9108539694884144, -5.589247009368157215, 74.99887465166234790 ) ) ;
#6281 = FACE_BOUND ( 'NONE', #16596, .T. ) ;
#6282 = ORIENTED_EDGE ( 'NONE', *, *, #28042, .F. ) ;
#6283 = FACE_OUTER_BOUND ( 'NONE', #2505, .T. ) ;
#6284 = DIRECTION ( 'NONE',  ( -0.000000000000000000, 0.000000000000000000, -1.000000000000000000 ) ) ;
#6285 = FACE_OUTER_BOUND ( 'NONE', #8277, .T. ) ;
#6287 = ORIENTED_EDGE ( 'NONE', *, *, #11206, .T. ) ;
#6286 = EDGE_LOOP ( 'NONE', ( #15963, #23267, #26064, #3538 ) ) ;
#6288 = CARTESIAN_POINT ( 'NONE',  ( 102.7763551498842816, 237.8836077948904517, -25.40199625708464382 ) ) ;
#6289 = ORIENTED_EDGE ( 'NONE', *, *, #5720, .T. ) ;
#6290 = DIRECTION ( 'NONE',  ( 0.000000000000000000, -1.000000000000000000, -1.214306433183764966E-16 ) ) ;
#6291 = ORIENTED_EDGE ( 'NONE', *, *, #19938, .T. ) ;
#6292 = VECTOR ( 'NONE', #1002, 1000.000000000000000 ) ;
#6293 = ORIENTED_EDGE ( 'NONE', *, *, #5428, .F. ) ;
#6294 = EDGE_CURVE ( 'NONE', #8492, #5793, #20064, .T. ) ;
#6295 = ORIENTED_EDGE ( 'NONE', *, *, #7225, .F. ) ;
#6296 = ORIENTED_EDGE ( 'NONE', *, *, #7625, .F. ) ;
#6297 = ORIENTED_EDGE ( 'NONE', *, *, #12021, .F. ) ;
#6298 = LINE ( 'NONE', #8323, #17324 ) ;
#6299 = ADVANCED_FACE ( 'NONE', ( #16203 ), #11469, .F. ) ;
#6300 = EDGE_CURVE ( 'NONE', #10546, #21766, #15634, .T. ) ;
#6301 = DIRECTION ( 'NONE',  ( 1.000000000000000000, 4.163336342344337027E-16, -0.000000000000000000 ) ) ;
#6302 = DIRECTION ( 'NONE',  ( 0.000000000000000000, -1.000000000000000000, 0.000000000000000000 ) ) ;
#6304 = CIRCLE ( 'NONE', #26029, 22.49999999999997868 ) ;
#6303 = CARTESIAN_POINT ( 'NONE',  ( -180.0000000000000284, -2.775557561562891982E-14, -70.00000000000001421 ) ) ;
#6305 = PRODUCT_DEFINITION ( 'UNKNOWN', '', #22120, #18087 ) ;
#6306 = DIRECTION ( 'NONE',  ( 0.000000000000000000, 0.000000000000000000, -1.000000000000000000 ) ) ;
#6307 = DIRECTION ( 'NONE',  ( -0.000000000000000000, -0.000000000000000000, -1.000000000000000000 ) ) ;
#6308 = VECTOR ( 'NONE', #20653, 1000.000000000000114 ) ;
#6309 = CARTESIAN_POINT ( 'NONE',  ( -236.2685473594162602, 81.43844187475562535, -14.99999999999999822 ) ) ;
#6310 = CARTESIAN_POINT ( 'NONE',  ( -24.72692578937659036, 129.2488030442671914, 16.96197069768293986 ) ) ;
#6311 = CARTESIAN_POINT ( 'NONE',  ( -209.9968669296227972, 60.57716416197344245, 21.99717788492469595 ) ) ;
#6312 = LINE ( 'NONE', #1581, #21602 ) ;
#6313 = FACE_OUTER_BOUND ( 'NONE', #15755, .T. ) ;
#6314 = ORIENTED_EDGE ( 'NONE', *, *, #10081, .F. ) ;
#6315 = CARTESIAN_POINT ( 'NONE',  ( -168.2126854711127635, 116.6621084685910574, 24.58429559685009380 ) ) ;
#6316 = DIRECTION ( 'NONE',  ( 1.000000000000000000, -1.832271836300406591E-15, 0.000000000000000000 ) ) ;
#6317 = VERTEX_POINT ( 'NONE', #540 ) ;
#6318 = APPLICATION_PROTOCOL_DEFINITION ( 'draft international standard', 'automotive_design', 1998, #23235 ) ;
#6319 = EDGE_CURVE ( 'NONE', #12718, #1480, #15781, .T. ) ;
#6320 = ORIENTED_EDGE ( 'NONE', *, *, #23299, .F. ) ;
#6321 = ORIENTED_EDGE ( 'NONE', *, *, #14801, .F. ) ;
#6322 = VECTOR ( 'NONE', #27537, 1000.000000000000000 ) ;
#6323 = EDGE_CURVE ( 'NONE', #27440, #5617, #23847, .T. ) ;
#6324 = CARTESIAN_POINT ( 'NONE',  ( 157.9999999999999716, 210.9684999699701393, 45.00000000000000000 ) ) ;
#6325 = LINE ( 'NONE', #6189, #9010 ) ;
#6326 = VECTOR ( 'NONE', #2309, 1000.000000000000227 ) ;
#6327 = ORIENTED_EDGE ( 'NONE', *, *, #1410, .F. ) ;
#6328 = ORIENTED_EDGE ( 'NONE', *, *, #26630, .T. ) ;
#6329 = CARTESIAN_POINT ( 'NONE',  ( 101.7779539752773275, 119.2876405402304982, -100.0000000000216716 ) ) ;
#6330 = CARTESIAN_POINT ( 'NONE',  ( 89.55286837137404632, 230.0961515142736573, 16.54242047486848932 ) ) ;
#6331 = EDGE_CURVE ( 'NONE', #5762, #14227, #24778, .T. ) ;
#6332 = CARTESIAN_POINT ( 'NONE',  ( 158.0000000000003979, 168.8424998498591663, -45.00000000000000000 ) ) ;
#6333 = ORIENTED_EDGE ( 'NONE', *, *, #4959, .F. ) ;
#6334 = CARTESIAN_POINT ( 'NONE',  ( -226.8383669992199430, 90.02672605029661668, 13.69137186706111997 ) ) ;
#6335 = VERTEX_POINT ( 'NONE', #24525 ) ;
#6336 = LINE ( 'NONE', #27739, #13471 ) ;
#6337 = EDGE_CURVE ( 'NONE', #3012, #14281, #16973, .T. ) ;
#6338 = CIRCLE ( 'NONE', #26066, 4.355764593064429313 ) ;
#6339 = DIRECTION ( 'NONE',  ( -0.2458199939946738577, -0.9693154958796741383, 0.000000000000000000 ) ) ;
#6340 = FACE_OUTER_BOUND ( 'NONE', #10827, .T. ) ;
#6341 = CARTESIAN_POINT ( 'NONE',  ( 157.4999999999998579, 193.6673124211760353, -45.00000000000000000 ) ) ;
#6342 = CIRCLE ( 'NONE', #2216, 75.00000000000002842 ) ;
#6343 = ORIENTED_EDGE ( 'NONE', *, *, #25057, .T. ) ;
#6344 = CARTESIAN_POINT ( 'NONE',  ( 157.9999999999998010, 236.5551250525490161, 45.00000000000000000 ) ) ;
#6345 = VECTOR ( 'NONE', #27258, 1000.000000000000227 ) ;
#6346 = CARTESIAN_POINT ( 'NONE',  ( 367.9108539694884144, -280.0000000000000568, 167.7200181511720132 ) ) ;
#6347 = DIRECTION ( 'NONE',  ( 1.000000000000000000, -0.000000000000000000, -0.000000000000000000 ) ) ;
#6348 = CARTESIAN_POINT ( 'NONE',  ( 25.90578987075423001, -14.95671475544977724, 45.00000000000000000 ) ) ;
#6349 = VERTEX_POINT ( 'NONE', #9588 ) ;
#6350 = EDGE_CURVE ( 'NONE', #20577, #1393, #922, .T. ) ;
#6351 = CARTESIAN_POINT ( 'NONE',  ( 157.9999999999997442, 254.1102501050980322, -45.00000000000000000 ) ) ;
#6352 = PLANE ( 'NONE',  #22645 ) ;
#6353 = DIRECTION ( 'NONE',  ( 1.000000000000000000, 0.000000000000000000, 0.000000000000000000 ) ) ;
#6354 = CARTESIAN_POINT ( 'NONE',  ( -229.6313009160351442, 91.61680614984454962, 13.11372941846348361 ) ) ;
#6355 = ORIENTED_EDGE ( 'NONE', *, *, #26523, .T. ) ;
#6356 = CARTESIAN_POINT ( 'NONE',  ( 158.0000000000006821, 140.7479997597746433, 45.00000000000000000 ) ) ;
#6357 = VERTEX_POINT ( 'NONE', #24815 ) ;
#6358 = EDGE_CURVE ( 'NONE', #24118, #13603, #15154, .T. ) ;
#6359 = CARTESIAN_POINT ( 'NONE',  ( 162.6509609271901411, 34.34969631929494938, -45.00000000000000000 ) ) ;
#6360 = VECTOR ( 'NONE', #11203, 1000.000000000000000 ) ;
#6361 = CARTESIAN_POINT ( 'NONE',  ( -175.2889320536586979, 112.8162159305347814, -27.79264103675363629 ) ) ;
#6362 = ORIENTED_EDGE ( 'NONE', *, *, #17811, .F. ) ;
#6363 = ORIENTED_EDGE ( 'NONE', *, *, #4122, .T. ) ;
#6364 = CARTESIAN_POINT ( 'NONE',  ( -112.7754610104328634, 70.85428810103185526, 82.84745292188917176 ) ) ;
#6365 = ORIENTED_EDGE ( 'NONE', *, *, #17792, .F. ) ;
#6366 = CIRCLE ( 'NONE', #24734, 22.49999999999997868 ) ;
#6367 = PRODUCT_DEFINITION_SHAPE ( 'NONE', 'NONE',  #28413 ) ;
#6368 = CARTESIAN_POINT ( 'NONE',  ( 158.0000000000007958, 128.7164997297464595, 45.00000000000000000 ) ) ;
#6369 = VECTOR ( 'NONE', #25558, 1000.000000000000000 ) ;
#6370 = ORIENTED_EDGE ( 'NONE', *, *, #18268, .T. ) ;
#6371 = ORIENTED_EDGE ( 'NONE', *, *, #16437, .T. ) ;
#6372 = CARTESIAN_POINT ( 'NONE',  ( 157.9999999999998295, 224.0157500150140208, 45.00000000000000000 ) ) ;
#6373 = AXIS2_PLACEMENT_3D ( 'NONE', #25580, #3746, #15114 ) ;
#6374 = ADVANCED_FACE ( 'NONE', ( #14744 ), #23499, .F. ) ;
#6375 = EDGE_CURVE ( 'NONE', #5668, #10085, #16617, .T. ) ;
#6376 = CARTESIAN_POINT ( 'NONE',  ( -40.00387671809203738, 149.2965004116384762, -45.00000000000000000 ) ) ;
#6377 = DIRECTION ( 'NONE',  ( 0.000000000000000000, 0.000000000000000000, 1.000000000000000000 ) ) ;
#6378 = LINE ( 'NONE', #26467, #27310 ) ;
#6379 = CARTESIAN_POINT ( 'NONE',  ( 158.0000000000005116, 158.8109998198309825, 45.00000000000000000 ) ) ;
#6380 = DIRECTION ( 'NONE',  ( 0.8660254037844432595, 0.4999999999999919509, -0.000000000000000000 ) ) ;
#6381 = CARTESIAN_POINT ( 'NONE',  ( -224.2911920753269897, 72.03214051461351630, -18.76861173148824591 ) ) ;
#6382 = EDGE_LOOP ( 'NONE', ( #26483, #21417, #14008, #23224 ) ) ;
#6383 = VECTOR ( 'NONE', #5368, 1000.000000000000000 ) ;
#6384 = CARTESIAN_POINT ( 'NONE',  ( 158.0000000000005116, 158.8109998198309825, 45.00000000000000000 ) ) ;
#6385 = CIRCLE ( 'NONE', #896, 19.99999999999998934 ) ;
#6386 = DIRECTION ( 'NONE',  ( 0.000000000000000000, -1.000000000000000000, 0.000000000000000000 ) ) ;
#6387 = CARTESIAN_POINT ( 'NONE',  ( 158.0000000000012221, 88.59049960963380954, 45.00000000000000000 ) ) ;
#6388 = DIRECTION ( 'NONE',  ( -0.7071067811865613395, -0.7071067811865335839, 0.000000000000000000 ) ) ;
#6389 = EDGE_LOOP ( 'NONE', ( #7718, #19393 ) ) ;
#6390 = EDGE_CURVE ( 'NONE', #17712, #14597, #19263, .T. ) ;
#6391 = CARTESIAN_POINT ( 'NONE',  ( 157.9999999999996305, 284.2047501951820436, 45.00000000000000000 ) ) ;
#6392 = AXIS2_PLACEMENT_3D ( 'NONE', #25404, #21658, #13059 ) ;
#6393 = CARTESIAN_POINT ( 'NONE',  ( 33.10302365956999182, 221.6666220619077876, 12.99999999999999822 ) ) ;
#6394 = FACE_OUTER_BOUND ( 'NONE', #1301, .T. ) ;
#6395 = DIRECTION ( 'NONE',  ( -0.9654425086906593956, 0.2448377981135679560, -0.08930405941493296806 ) ) ;
#6396 = CARTESIAN_POINT ( 'NONE',  ( 157.9999999999996305, 286.2047501951820436, -45.00000000000000000 ) ) ;
#6397 = FILL_AREA_STYLE_COLOUR ( '', #4210 ) ;
#6398 = ORIENTED_EDGE ( 'NONE', *, *, #3991, .F. ) ;
#6400 = ADVANCED_FACE ( 'NONE', ( #10429 ), #27792, .F. ) ;
#6399 = VECTOR ( 'NONE', #7762, 1000.000000000000227 ) ;
#6401 = SPHERICAL_SURFACE ( 'NONE', #22626, 5.000000000000000000 ) ;
#6402 = ORIENTED_EDGE ( 'NONE', *, *, #18143, .T. ) ;
#6403 = LINE ( 'NONE', #10863, #6687 ) ;
#6404 = VERTEX_POINT ( 'NONE', #23079 ) ;
#6405 = EDGE_CURVE ( 'NONE', #12131, #17425, #1369, .T. ) ;
#6406 = ORIENTED_EDGE ( 'NONE', *, *, #28394, .F. ) ;
#6407 = CARTESIAN_POINT ( 'NONE',  ( -76.25760768171835480, 219.6666220619077876, -13.00000000000000000 ) ) ;
#6408 = VECTOR ( 'NONE', #27165, 1000.000000000000114 ) ;
#6409 = ORIENTED_EDGE ( 'NONE', *, *, #22288, .F. ) ;
#6410 =( BOUNDED_SURFACE ( )  B_SPLINE_SURFACE ( 3, 2, ( 
 ( #6553, #15189, #21922 ),
 ( #2228, #13315, #22064 ),
 ( #19764, #8851, #19908 ),
 ( #2372, #17609, #11154 ),
 ( #15614, #2094, #26083 ),
 ( #235, #8997, #4253 ),
 ( #28090, #21786, #17750 ),
 ( #23799, #26364, #24357 ),
 ( #6694, #5062, #19626 ),
 ( #2912, #11697, #8435 ) ),
 .UNSPECIFIED., .F., .F., .F. ) 
 B_SPLINE_SURFACE_WITH_KNOTS ( ( 4, 2, 2, 2, 4 ),
 ( 3, 3 ),
 ( 0.000000000000000000, 0.003993085574633960591, 0.007986171149267921182, 0.01197925672390188177, 0.01597234229853584236 ),
 ( 0.000000000000000000, 1.000000000000000000 ),
 .UNSPECIFIED. ) 
 GEOMETRIC_REPRESENTATION_ITEM ( )  RATIONAL_B_SPLINE_SURFACE ( (
 ( 1.000000000000000000, 0.7071067811865441310, 1.000000000000000000),
 ( 1.000000000000000000, 0.6986941146418389481, 1.000000000000000000),
 ( 1.000000000000000000, 0.6922065170597959671, 1.000000000000000000),
 ( 1.000000000000000000, 0.6834952607772883937, 1.000000000000000000),
 ( 1.000000000000000000, 0.6812778029564220406, 1.000000000000000000),
 ( 1.000000000000000000, 0.6812778029564220406, 1.000000000000000000),
 ( 1.000000000000000000, 0.6834952607749916753, 1.000000000000000000),
 ( 1.000000000000000000, 0.6922065170620920194, 1.000000000000000000),
 ( 1.000000000000000000, 0.6986941146401082214, 1.000000000000000000),
 ( 1.000000000000000000, 0.7071067811865499042, 1.000000000000000000) ) ) 
 REPRESENTATION_ITEM ( '' )  SURFACE ( )  );
#6411 = EDGE_LOOP ( 'NONE', ( #1218, #9269, #21436, #4197 ) ) ;
#6412 = CARTESIAN_POINT ( 'NONE',  ( -241.9743096803475453, -91.18033988749901653, -17.46154499483315448 ) ) ;
#6413 = DIRECTION ( 'NONE',  ( -0.000000000000000000, -0.000000000000000000, -1.000000000000000000 ) ) ;
#6414 = CARTESIAN_POINT ( 'NONE',  ( -212.5524510162168212, -218.0941723687616900, 93.50253975917524940 ) ) ;
#6415 = AXIS2_PLACEMENT_3D ( 'NONE', #17916, #26667, #13768 ) ;
#6416 = FACE_OUTER_BOUND ( 'NONE', #5530, .T. ) ;
#6417 = ADVANCED_FACE ( 'NONE', ( #18764 ), #27510, .F. ) ;
#6418 = CARTESIAN_POINT ( 'NONE',  ( -175.0000000000000000, -120.0000000000001847, -69.99999999999998579 ) ) ;
#6419 = CARTESIAN_POINT ( 'NONE',  ( 209.9999999999999432, -280.0000000000000000, 99.99999999999991473 ) ) ;
#6420 = CARTESIAN_POINT ( 'NONE',  ( 158.0000000000015632, 55.98812451204224061, 45.00000000000000000 ) ) ;
#6421 = CARTESIAN_POINT ( 'NONE',  ( -42.99650729631200363, 71.03850157808263077, 99.00000000000000000 ) ) ;
#6422 = CARTESIAN_POINT ( 'NONE',  ( 158.0000000000012221, 90.59049960963380954, 45.00000000000000000 ) ) ;
#6423 = FACE_OUTER_BOUND ( 'NONE', #27077, .T. ) ;
#6424 = CARTESIAN_POINT ( 'NONE',  ( 158.0000000000009379, 116.1771246922112653, 45.00000000000000000 ) ) ;
#6425 = FACE_OUTER_BOUND ( 'NONE', #9155, .T. ) ;
#6426 = CARTESIAN_POINT ( 'NONE',  ( 157.4999999999998579, 123.4468122109788482, 45.00000000000000000 ) ) ;
#6427 = EDGE_LOOP ( 'NONE', ( #13964, #19714, #18868, #25130 ) ) ;
#6428 = FACE_OUTER_BOUND ( 'NONE', #15933, .T. ) ;
#6429 = AXIS2_PLACEMENT_3D ( 'NONE', #24801, #2809, #5390 ) ;
#6430 = LINE ( 'NONE', #21513, #11479 ) ;
#6431 = CARTESIAN_POINT ( 'NONE',  ( 158.0000000000008242, 126.2086247222394206, -45.00000000000000000 ) ) ;
#6432 = CARTESIAN_POINT ( 'NONE',  ( 107.6443576357609828, 207.6802486446758564, -150.2059422892478722 ) ) ;
#6433 = VERTEX_POINT ( 'NONE', #25227 ) ;
#6434 = EDGE_CURVE ( 'NONE', #26356, #6230, #25092, .T. ) ;
#6435 = EDGE_CURVE ( 'NONE', #8321, #22143, #5404, .T. ) ;
#6436 = CIRCLE ( 'NONE', #18, 5.000000000000000888 ) ;
#6437 = CARTESIAN_POINT ( 'NONE',  ( 92.04920872067096127, 230.5961997032265174, -17.50980340464030505 ) ) ;
#6438 = VERTEX_POINT ( 'NONE', #3667 ) ;
#6439 = CARTESIAN_POINT ( 'NONE',  ( 157.4999999999996305, 288.9665627064425735, 45.00000000000000000 ) ) ;
#6440 = ORIENTED_EDGE ( 'NONE', *, *, #20583, .T. ) ;
#6441 = ORIENTED_EDGE ( 'NONE', *, *, #18188, .F. ) ;
#6442 = EDGE_LOOP ( 'NONE', ( #23463, #26285, #12295, #13588 ) ) ;
#6443 = ORIENTED_EDGE ( 'NONE', *, *, #6541, .T. ) ;
#6444 = EDGE_LOOP ( 'NONE', ( #2742, #21071, #25603, #21574 ) ) ;
#6445 = CARTESIAN_POINT ( 'NONE',  ( 158.0000000000003126, 176.3661248723802828, -45.00000000000000000 ) ) ;
#6446 = AXIS2_PLACEMENT_3D ( 'NONE', #13045, #383, #9145 ) ;
#6447 = DIRECTION ( 'NONE',  ( -1.000000000000000000, 0.000000000000000000, 0.000000000000000000 ) ) ;
#6448 = DIRECTION ( 'NONE',  ( 0.000000000000000000, -1.000000000000000000, 0.000000000000000000 ) ) ;
#6449 = VECTOR ( 'NONE', #13078, 1000.000000000000000 ) ;
#6450 = CARTESIAN_POINT ( 'NONE',  ( 158.0000000000003695, 171.3503748573662051, 45.00000000000000000 ) ) ;
#6451 = DIRECTION ( 'NONE',  ( 1.000000000000000000, 8.673617379884036705E-17, 0.000000000000000000 ) ) ;
#6452 = ADVANCED_FACE ( 'NONE', ( #9864 ), #7712, .F. ) ;
#6453 = FACE_OUTER_BOUND ( 'NONE', #23510, .T. ) ;
#6454 = LINE ( 'NONE', #19671, #1134 ) ;
#6455 = CARTESIAN_POINT ( 'NONE',  ( 410.1240808061609755, 61.15703788601290114, -683.1631314933625845 ) ) ;
#6456 = CARTESIAN_POINT ( 'NONE',  ( -233.7109140654491171, 78.16279237795507129, -15.26611692692816824 ) ) ;
#6457 = CARTESIAN_POINT ( 'NONE',  ( -68.57415822541635464, 80.97823757117562593, 95.00000000000000000 ) ) ;
#6458 = DIRECTION ( 'NONE',  ( 0.000000000000000000, 0.000000000000000000, -1.000000000000000000 ) ) ;
#6459 = DIRECTION ( 'NONE',  ( -1.000000000000000000, 0.000000000000000000, 0.000000000000000000 ) ) ;
#6460 = ADVANCED_FACE ( 'NONE', ( #6394 ), #15173, .F. ) ;
#6461 = PLANE ( 'NONE',  #14824 ) ;
#6463 = ORIENTED_EDGE ( 'NONE', *, *, #24834, .T. ) ;
#6462 = ORIENTED_EDGE ( 'NONE', *, *, #25990, .T. ) ;
#6464 = CARTESIAN_POINT ( 'NONE',  ( -224.8814028220360797, 87.10059759008312597, -16.59626922761215795 ) ) ;
#6465 = EDGE_CURVE ( 'NONE', #13456, #11112, #21094, .T. ) ;
#6466 = PRESENTATION_LAYER_ASSIGNMENT (  '', '', ( #4160 ) ) ;
#6467 = EDGE_CURVE ( 'NONE', #9950, #15333, #14681, .T. ) ;
#6468 = LINE ( 'NONE', #13372, #13114 ) ;
#6469 = VERTEX_POINT ( 'NONE', #22046 ) ;
#6470 = SHAPE_DEFINITION_REPRESENTATION ( #21748, #26803 ) ;
#6471 = ORIENTED_EDGE ( 'NONE', *, *, #17845, .T. ) ;
#6472 = VERTEX_POINT ( 'NONE', #10855 ) ;
#6473 = VECTOR ( 'NONE', #23994, 1000.000000000000000 ) ;
#6474 = CARTESIAN_POINT ( 'NONE',  ( 157.9999999999997442, 254.1102501050980322, 45.00000000000000000 ) ) ;
#6475 = DIRECTION ( 'NONE',  ( 0.9985600561963489108, -0.05364526231778980747, 0.000000000000000000 ) ) ;
#6476 = ORIENTED_EDGE ( 'NONE', *, *, #15072, .T. ) ;
#6477 = CARTESIAN_POINT ( 'NONE',  ( 98.15430812615089451, 116.0637945823775112, -78.75000000033432457 ) ) ;
#6478 = CARTESIAN_POINT ( 'NONE',  ( -162.6958652128487586, 119.3823555589419669, -22.14487429185738421 ) ) ;
#6479 = ORIENTED_EDGE ( 'NONE', *, *, #17885, .T. ) ;
#6480 = CARTESIAN_POINT ( 'NONE',  ( -211.3786312416644364, 87.57134810217682741, 24.25168111795433390 ) ) ;
#6481 = ORIENTED_EDGE ( 'NONE', *, *, #27821, .F. ) ;
#6482 = DIRECTION ( 'NONE',  ( 1.321694076934710155E-16, -1.000000000000000000, 0.000000000000000000 ) ) ;
#6483 = AXIS2_PLACEMENT_3D ( 'NONE', #101, #24101, #19919 ) ;
#6484 = CARTESIAN_POINT ( 'NONE',  ( -84.36128592734598897, 105.7287271543808487, -145.0000000000000000 ) ) ;
#6485 = CARTESIAN_POINT ( 'NONE',  ( 160.5798347354847238, 204.3213570346847519, -150.9608879355640170 ) ) ;
#6486 = AXIS2_PLACEMENT_3D ( 'NONE', #19894, #19327, #10857 ) ;
#6487 = CARTESIAN_POINT ( 'NONE',  ( 158.0000000000014495, 66.01962454207041731, -45.00000000000000000 ) ) ;
#6488 = VECTOR ( 'NONE', #17209, 1000.000000000000000 ) ;
#6489 = EDGE_CURVE ( 'NONE', #8537, #1982, #6251, .T. ) ;
#6490 = ORIENTED_EDGE ( 'NONE', *, *, #3085, .T. ) ;
#6491 = CARTESIAN_POINT ( 'NONE',  ( 187.4999999999996305, 133.0668745871126930, 36.86484227207694886 ) ) ;
#6492 = LINE ( 'NONE', #14988, #17920 ) ;
#6493 = DIRECTION ( 'NONE',  ( -0.000000000000000000, -0.000000000000000000, -1.000000000000000000 ) ) ;
#6494 = DIRECTION ( 'NONE',  ( 0.000000000000000000, 1.000000000000000000, 0.000000000000000000 ) ) ;
#6495 = ORIENTED_EDGE ( 'NONE', *, *, #12897, .T. ) ;
#6496 = CARTESIAN_POINT ( 'NONE',  ( -211.8239278721113408, -220.0000000000001421, -106.9797831932409622 ) ) ;
#6497 = EDGE_CURVE ( 'NONE', #27076, #2009, #8715, .T. ) ;
#6498 = DIRECTION ( 'NONE',  ( 0.8916010070300078860, -0.4528218681369923782, 0.000000000000000000 ) ) ;
#6499 = CARTESIAN_POINT ( 'NONE',  ( -24.92338318254761020, 127.6681916698425567, -145.0000000000000000 ) ) ;
#6500 = ORIENTED_EDGE ( 'NONE', *, *, #19957, .T. ) ;
#6501 = ORIENTED_EDGE ( 'NONE', *, *, #3309, .F. ) ;
#6502 = EDGE_CURVE ( 'NONE', #5842, #6860, #4093, .T. ) ;
#6503 = AXIS2_PLACEMENT_3D ( 'NONE', #19883, #15734, #20168 ) ;
#6504 = CARTESIAN_POINT ( 'NONE',  ( -216.4421519707229891, 141.6000904446840707, -15.00000000000000000 ) ) ;
#6505 = CARTESIAN_POINT ( 'NONE',  ( -188.6691793476254020, 104.3291597953724761, -32.37965609178030491 ) ) ;
#6506 = ORIENTED_EDGE ( 'NONE', *, *, #3861, .F. ) ;
#6507 = AXIS2_PLACEMENT_3D ( 'NONE', #891, #7223, #18145 ) ;
#6508 = CARTESIAN_POINT ( 'NONE',  ( 158.0000000000002842, 180.8739998798873501, 45.00000000000000000 ) ) ;
#6509 = ORIENTED_EDGE ( 'NONE', *, *, #23129, .F. ) ;
#6510 = DIRECTION ( 'NONE',  ( 0.000000000000000000, 0.000000000000000000, -1.000000000000000000 ) ) ;
#6511 = VECTOR ( 'NONE', #21773, 1000.000000000000000 ) ;
#6512 = FACE_OUTER_BOUND ( 'NONE', #24004, .T. ) ;
#6513 = VERTEX_POINT ( 'NONE', #26209 ) ;
#6514 = ORIENTED_EDGE ( 'NONE', *, *, #12535, .F. ) ;
#6515 = CARTESIAN_POINT ( 'NONE',  ( -13.43082424514546069, 129.5962963036035944, 16.85783026249312400 ) ) ;
#6516 = CARTESIAN_POINT ( 'NONE',  ( -210.0000000000000568, -220.0000000000000853, 110.0000000000000284 ) ) ;
#6517 = CARTESIAN_POINT ( 'NONE',  ( -41.54405845664282282, 46.26118624020713099, -45.00000000000000000 ) ) ;
#6518 = DIRECTION ( 'NONE',  ( 0.000000000000000000, -1.000000000000000000, 0.000000000000000000 ) ) ;
#6519 = DIRECTION ( 'NONE',  ( 0.5457381880580516320, -0.8379557447115657531, 0.000000000000000000 ) ) ;
#6520 = AXIS2_PLACEMENT_3D ( 'NONE', #11696, #16420, #23015 ) ;
#6521 = LINE ( 'NONE', #19878, #5068 ) ;
#6522 = DIRECTION ( 'NONE',  ( 0.000000000000000000, 0.000000000000000000, -1.000000000000000000 ) ) ;
#6523 = ADVANCED_FACE ( 'NONE', ( #28216 ), #27929, .T. ) ;
#6524 = ORIENTED_EDGE ( 'NONE', *, *, #28294, .T. ) ;
#6525 = AXIS2_PLACEMENT_3D ( 'NONE', #610, #13832, #22998 ) ;
#6526 = LINE ( 'NONE', #21762, #21394 ) ;
#6527 = CARTESIAN_POINT ( 'NONE',  ( 157.4999999999998579, 130.9704372334999789, -45.00000000000000000 ) ) ;
#6529 = LINE ( 'NONE', #8690, #1769 ) ;
#6528 = AXIS2_PLACEMENT_3D ( 'NONE', #22127, #4738, #4315 ) ;
#6530 = PLANE ( 'NONE',  #15784 ) ;
#6531 = CARTESIAN_POINT ( 'NONE',  ( 157.4999999999998579, 193.6673124211760353, 45.00000000000000000 ) ) ;
#6532 = EDGE_LOOP ( 'NONE', ( #14267, #27352, #15892, #7949 ) ) ;
#6533 = CARTESIAN_POINT ( 'NONE',  ( -160.0000000000000284, 59.99999999999994316, -70.00000000000001421 ) ) ;
#6534 = CIRCLE ( 'NONE', #26731, 6.000000000000005329 ) ;
#6535 = CARTESIAN_POINT ( 'NONE',  ( -125.2895325436294058, 200.2180533211638362, -15.00000000000000000 ) ) ;
#6536 = CARTESIAN_POINT ( 'NONE',  ( 158.0000000000005116, 158.8109998198309825, 45.00000000000000000 ) ) ;
#6537 = CARTESIAN_POINT ( 'NONE',  ( 158.0000000000001421, 191.4133749174225443, 45.00000000000000000 ) ) ;
#6538 = CARTESIAN_POINT ( 'NONE',  ( 158.0000000000001137, 193.9212499249295831, 45.00000000000000000 ) ) ;
#6539 = DIRECTION ( 'NONE',  ( -1.000000000000000000, -0.000000000000000000, -0.000000000000000000 ) ) ;
#6540 = VERTEX_POINT ( 'NONE', #12738 ) ;
#6541 = EDGE_CURVE ( 'NONE', #2227, #12260, #17591, .T. ) ;
#6542 = CARTESIAN_POINT ( 'NONE',  ( -225.9974328972257069, 72.66572410194898168, 17.86196565642464051 ) ) ;
#6543 = ORIENTED_EDGE ( 'NONE', *, *, #11101, .F. ) ;
#6544 = EDGE_CURVE ( 'NONE', #9950, #20572, #21908, .T. ) ;
#6545 = CARTESIAN_POINT ( 'NONE',  ( 157.9999999999998010, 238.5551250525490161, -45.00000000000000000 ) ) ;
#6546 = ORIENTED_EDGE ( 'NONE', *, *, #19029, .F. ) ;
#6547 = VECTOR ( 'NONE', #4849, 1000.000000000000000 ) ;
#6548 = ORIENTED_EDGE ( 'NONE', *, *, #12748, .T. ) ;
#6549 = CARTESIAN_POINT ( 'NONE',  ( 109.9999999999999005, 3.816391647148972452E-14, -25.00000000000000000 ) ) ;
#6550 = EDGE_LOOP ( 'NONE', ( #5728, #7123, #5723, #27554 ) ) ;
#6551 = ORIENTED_EDGE ( 'NONE', *, *, #28012, .F. ) ;
#6552 = VECTOR ( 'NONE', #1431, 1000.000000000000000 ) ;
#6553 = CARTESIAN_POINT ( 'NONE',  ( -227.8378063125350650, 130.6400894613935293, 13.00000000000000000 ) ) ;
#6554 = ADVANCED_FACE ( 'NONE', ( #4236 ), #13024, .F. ) ;
#6555 = CARTESIAN_POINT ( 'NONE',  ( -274.7557459110829541, -165.0000000000001421, 86.12025961983462707 ) ) ;
#6556 = CARTESIAN_POINT ( 'NONE',  ( 89.99999999999988631, 240.0000000000000284, 6.270166537925822681 ) ) ;
#6557 = CIRCLE ( 'NONE', #9314, 4.999999999999992895 ) ;
#6558 = EDGE_CURVE ( 'NONE', #5346, #18031, #21477, .T. ) ;
#6559 = CIRCLE ( 'NONE', #10797, 7.500000000000007105 ) ;
#6560 = CARTESIAN_POINT ( 'NONE',  ( 158.0000000000015916, 53.48024950453520177, -45.00000000000000000 ) ) ;
#6561 = CARTESIAN_POINT ( 'NONE',  ( -254.3350114625770289, -91.18033988749901653, 0.000000000000000000 ) ) ;
#6562 = CARTESIAN_POINT ( 'NONE',  ( -59.48697296830715686, 2.336311854928213219E-15, 99.00000000000000000 ) ) ;
#6563 = CARTESIAN_POINT ( 'NONE',  ( 157.9999999999999432, 213.4763749774776045, 45.00000000000000000 ) ) ;
#6564 = CARTESIAN_POINT ( 'NONE',  ( -210.7125095212385020, 88.79578285577181873, -22.86806245198074450 ) ) ;
#6565 = CARTESIAN_POINT ( 'NONE',  ( -160.0000000000000284, 59.99999999999994316, 45.00000000000000000 ) ) ;
#6566 = CARTESIAN_POINT ( 'NONE',  ( 158.0000000000016200, 52.97237449702815582, -45.00000000000000000 ) ) ;
#6567 = EDGE_CURVE ( 'NONE', #17968, #27440, #5875, .T. ) ;
#6568 = LINE ( 'NONE', #13467, #10167 ) ;
#6569 = CARTESIAN_POINT ( 'NONE',  ( 158.0000000000015064, 63.00387452705633251, 45.00000000000000000 ) ) ;
#6570 = VERTEX_POINT ( 'NONE', #1934 ) ;
#6571 = VECTOR ( 'NONE', #23164, 1000.000000000000000 ) ;
#6572 = CARTESIAN_POINT ( 'NONE',  ( 157.9999999999998863, 218.4921249924925348, 45.00000000000000000 ) ) ;
#6573 = CONICAL_SURFACE ( 'NONE', #17127, 5.999999999999977796, 1.029744258676652091 ) ;
#6574 = CARTESIAN_POINT ( 'NONE',  ( 134.9999999999998579, 220.0000000000000284, -119.9999999999999858 ) ) ;
#6575 = CARTESIAN_POINT ( 'NONE',  ( 109.9999999999999147, 140.0000000000000000, 45.00000000000000000 ) ) ;
#6576 = DIRECTION ( 'NONE',  ( -0.8916010070299268397, 0.4528218681371523058, 0.000000000000000000 ) ) ;
#6577 = VECTOR ( 'NONE', #6846, 1000.000000000000000 ) ;
#6578 = ORIENTED_EDGE ( 'NONE', *, *, #21278, .T. ) ;
#6579 = LINE ( 'NONE', #24114, #10229 ) ;
#6580 = ORIENTED_EDGE ( 'NONE', *, *, #24671, .F. ) ;
#6581 =( NAMED_UNIT ( * ) SI_UNIT ( $, .STERADIAN. ) SOLID_ANGLE_UNIT ( ) );
#6582 = ORIENTED_EDGE ( 'NONE', *, *, #12436, .T. ) ;
#6583 = EDGE_LOOP ( 'NONE', ( #3421, #22094, #2246, #18460 ) ) ;
#6584 = ORIENTED_EDGE ( 'NONE', *, *, #338, .F. ) ;
#6585 = VERTEX_POINT ( 'NONE', #19469 ) ;
#6586 = AXIS2_PLACEMENT_3D ( 'NONE', #23874, #6626, #24017 ) ;
#6587 = DIRECTION ( 'NONE',  ( -0.8916010070293584056, 0.4528218681382713551, 0.000000000000000000 ) ) ;
#6588 = VECTOR ( 'NONE', #5487, 1000.000000000000000 ) ;
#6589 = CYLINDRICAL_SURFACE ( 'NONE', #5493, 5.999999999999991118 ) ;
#6590 = CIRCLE ( 'NONE', #4294, 6.204828372381208546 ) ;
#6591 = UNCERTAINTY_MEASURE_WITH_UNIT (LENGTH_MEASURE( 1.000000000000000082E-05 ), #17884, 'distance_accuracy_value', 'NONE');
#6592 = CARTESIAN_POINT ( 'NONE',  ( 156.4999999999998579, 220.0000000000000284, 99.00000000000001421 ) ) ;
#6593 = EDGE_CURVE ( 'NONE', #18456, #5833, #8636, .T. ) ;
#6594 = CARTESIAN_POINT ( 'NONE',  ( -205.1716483941798401, 60.34345434848681577, 21.58965668827011442 ) ) ;
#6595 = CARTESIAN_POINT ( 'NONE',  ( 109.9999999999999147, 140.0000000000000000, -45.00000000000000000 ) ) ;
#6596 = CARTESIAN_POINT ( 'NONE',  ( -180.0000000000000284, -70.00000000000004263, 100.0000000000000142 ) ) ;
#6597 = CARTESIAN_POINT ( 'NONE',  ( 158.0000000000014211, 70.52749954957745615, 45.00000000000000000 ) ) ;
#6598 = CARTESIAN_POINT ( 'NONE',  ( -26.22291647523108438, 23.54903675176048594, 45.00000000000000000 ) ) ;
#6599 = ADVANCED_FACE ( 'NONE', ( #504 ), #2279, .F. ) ;
#6600 = DIRECTION ( 'NONE',  ( 0.8660254037844363761, -0.5000000000000039968, 0.000000000000000000 ) ) ;
#6601 = CARTESIAN_POINT ( 'NONE',  ( -231.0575465263486308, 75.69719229554537776, -15.88027955539508440 ) ) ;
#6602 = CARTESIAN_POINT ( 'NONE',  ( 157.4999999999998295, 226.2696875187675118, -45.00000000000000000 ) ) ;
#6603 = CARTESIAN_POINT ( 'NONE',  ( 157.4999999999998579, 128.4625622259929401, 45.00000000000000000 ) ) ;
#6604 = CARTESIAN_POINT ( 'NONE',  ( -177.8141338791984651, 110.9804198039069263, 30.03957269548647346 ) ) ;
#6605 = DIRECTION ( 'NONE',  ( 0.4528218681373908372, -0.8916010070298056034, 0.000000000000000000 ) ) ;
#6607 = EDGE_LOOP ( 'NONE', ( #20787, #21320, #14748, #24217 ) ) ;
#6606 = VERTEX_POINT ( 'NONE', #11286 ) ;
#6608 = AXIS2_PLACEMENT_3D ( 'NONE', #21756, #23625, #26054 ) ;
#6609 = CARTESIAN_POINT ( 'NONE',  ( -232.7323212076349535, 91.52112961950480496, -14.99999999999997513 ) ) ;
#6610 = PRODUCT ( 'Drive Gear', 'Drive Gear', '', ( #25859 ) ) ;
#6611 = ORIENTED_EDGE ( 'NONE', *, *, #4319, .T. ) ;
#6612 = APPLICATION_PROTOCOL_DEFINITION ( 'draft international standard', 'automotive_design', 1998, #18281 ) ;
#6613 = AXIS2_PLACEMENT_3D ( 'NONE', #16853, #4047, #2038 ) ;
#6614 = ORIENTED_EDGE ( 'NONE', *, *, #28115, .F. ) ;
#6615 = EDGE_LOOP ( 'NONE', ( #17187, #15860, #25463, #15884 ) ) ;
#6616 = CARTESIAN_POINT ( 'NONE',  ( -138.6428522700808230, 66.54464929955099706, 83.00000000000001421 ) ) ;
#6617 = ADVANCED_FACE ( 'NONE', ( #26481 ), #788, .F. ) ;
#6618 = DIRECTION ( 'NONE',  ( 0.4528218681379115873, 0.8916010070295411483, -0.000000000000000000 ) ) ;
#6619 = EDGE_LOOP ( 'NONE', ( #1726, #7376, #16041, #18394 ) ) ;
#6620 = CARTESIAN_POINT ( 'NONE',  ( 100.5794065448618255, 118.1137289703157336, -99.99999999995674216 ) ) ;
#6621 = CARTESIAN_POINT ( 'NONE',  ( -189.8086322075389774, 92.49158130768422836, -13.00000000000000000 ) ) ;
#6622 = ORIENTED_EDGE ( 'NONE', *, *, #13788, .F. ) ;
#6623 = EDGE_CURVE ( 'NONE', #19117, #13806, #217, .T. ) ;
#6624 = CARTESIAN_POINT ( 'NONE',  ( -210.7121506535087576, 88.79643741746845365, 22.86845985951527993 ) ) ;
#6625 = AXIS2_PLACEMENT_3D ( 'NONE', #10238, #18995, #5916 ) ;
#6626 = DIRECTION ( 'NONE',  ( -0.000000000000000000, 1.000000000000000000, -1.387778780781445429E-16 ) ) ;
#6627 = ADVANCED_FACE ( 'NONE', ( #26632 ), #7255, .F. ) ;
#6628 = ADVANCED_FACE ( 'NONE', ( #2645 ), #4938, .F. ) ;
#6629 = B_SPLINE_CURVE_WITH_KNOTS ( 'NONE', 3,
 ( #25560, #10344, #23413, #8046, #18680, #22994, #3444, #14807, #3869, #5883, #12513, #16536, #9790, #18545, #27292, #21256, #5462, #1577, #14246, #3299, #1156, #25285, #23136, #12237, #17658, #2139, #13222, #6172, #21539, #14949, #23702, #13084, #8474, #6601, #19246, #17231, #21966, #6456, #4008, #11057, #6309, #15087 ),
 .UNSPECIFIED., .F., .F.,
 ( 4, 2, 2, 2, 2, 2, 2, 2, 2, 2, 2, 2, 2, 2, 2, 2, 2, 2, 2, 2, 4 ),
 ( 0.000000000000000000, 0.001589323840935409323, 0.003178647681870818646, 0.006357295363741637291, 0.007946619204677041193, 0.009535943045612444227, 0.01271459072748320866, 0.01907188609122478784, 0.02225053377309557309, 0.02542918145496636181, 0.02860782913683715054, 0.03019715297777251714, 0.03178647681870788028, 0.03496512450057859961, 0.03655444834151396621, 0.03814377218244931894, 0.04132241986431998276, 0.04291174370525530773, 0.04450106754619062577, 0.04767971522806119938, 0.05085836290993178688 ),
 .UNSPECIFIED. ) ;
#6630 = ADVANCED_FACE ( 'NONE', ( #11431 ), #11722, .F. ) ;
#6631 = DIRECTION ( 'NONE',  ( 1.000000000000000000, 0.000000000000000000, -0.000000000000000000 ) ) ;
#6632 = VECTOR ( 'NONE', #20498, 1000.000000000000114 ) ;
#6633 = CARTESIAN_POINT ( 'NONE',  ( 158.9581838007524084, 201.9414044957390786, -149.7704424372630001 ) ) ;
#6634 = EDGE_LOOP ( 'NONE', ( #4485, #16006, #25241, #26036 ) ) ;
#6635 = CARTESIAN_POINT ( 'NONE',  ( 217.4999999999996305, 194.4107529906318064, -75.35061095560291733 ) ) ;
#6636 = CARTESIAN_POINT ( 'NONE',  ( 164.9999999999998579, 220.0000000000000284, -169.9999999999999716 ) ) ;
#6637 = DIRECTION ( 'NONE',  ( -0.000000000000000000, 0.000000000000000000, -1.000000000000000000 ) ) ;
#6638 = LINE ( 'NONE', #11242, #12153 ) ;
#6639 = EDGE_LOOP ( 'NONE', ( #18430, #1525, #27539, #28121 ) ) ;
#6640 = CARTESIAN_POINT ( 'NONE',  ( -210.6511289989136912, -220.0000000000000568, -108.6306965739821067 ) ) ;
#6641 = LINE ( 'NONE', #11246, #20804 ) ;
#6642 = DIRECTION ( 'NONE',  ( -0.000000000000000000, -0.000000000000000000, -1.000000000000000000 ) ) ;
#6643 = ORIENTED_EDGE ( 'NONE', *, *, #24293, .F. ) ;
#6644 = AXIS2_PLACEMENT_3D ( 'NONE', #12015, #20759, #26808 ) ;
#6645 = ORIENTED_EDGE ( 'NONE', *, *, #12584, .T. ) ;
#6646 = VECTOR ( 'NONE', #3579, 1000.000000000000000 ) ;
#6647 = DIRECTION ( 'NONE',  ( 0.000000000000000000, -1.000000000000000000, 0.000000000000000000 ) ) ;
#6648 = CARTESIAN_POINT ( 'NONE',  ( -194.8905955746074881, 99.56818556745220405, -32.54511976914040616 ) ) ;
#6649 = ORIENTED_EDGE ( 'NONE', *, *, #9750, .F. ) ;
#6650 = AXIS2_PLACEMENT_3D ( 'NONE', #16028, #20322, #11432 ) ;
#6651 = ORIENTED_EDGE ( 'NONE', *, *, #16592, .F. ) ;
#6652 = CARTESIAN_POINT ( 'NONE',  ( 232.4999999999996305, 133.0668745871126930, -30.83984227207694317 ) ) ;
#6653 = EDGE_CURVE ( 'NONE', #14756, #3239, #5485, .T. ) ;
#6654 = EDGE_CURVE ( 'NONE', #2475, #19162, #650, .T. ) ;
#6655 = DIRECTION ( 'NONE',  ( 0.000000000000000000, -0.000000000000000000, 1.000000000000000000 ) ) ;
#6656 = ORIENTED_EDGE ( 'NONE', *, *, #16032, .T. ) ;
#6657 = ORIENTED_EDGE ( 'NONE', *, *, #1533, .F. ) ;
#6658 = LINE ( 'NONE', #26464, #7018 ) ;
#6659 = EDGE_CURVE ( 'NONE', #8035, #9517, #6955, .T. ) ;
#6660 = EDGE_CURVE ( 'NONE', #7521, #6404, #22192, .T. ) ;
#6661 = FACE_OUTER_BOUND ( 'NONE', #13997, .T. ) ;
#6662 = DIRECTION ( 'NONE',  ( -1.000000000000000000, 0.000000000000000000, 0.000000000000000000 ) ) ;
#6663 = DIRECTION ( 'NONE',  ( 0.3102637045530823312, 0.9506505318133460225, 0.000000000000000000 ) ) ;
#6664 = CARTESIAN_POINT ( 'NONE',  ( 158.0000000000008811, 121.1928747072253572, -45.00000000000000000 ) ) ;
#6665 = AXIS2_PLACEMENT_3D ( 'NONE', #18059, #16055, #20348 ) ;
#6666 = CARTESIAN_POINT ( 'NONE',  ( -272.0365926943243835, -170.1453898595840144, 103.5646192279123170 ) ) ;
#6667 = CARTESIAN_POINT ( 'NONE',  ( 157.9999999999996305, 281.6968751876750616, 45.00000000000000000 ) ) ;
#6668 = ORIENTED_EDGE ( 'NONE', *, *, #27676, .F. ) ;
#6669 = FACE_OUTER_BOUND ( 'NONE', #11408, .T. ) ;
#6670 = VECTOR ( 'NONE', #13010, 1000.000000000000000 ) ;
#6671 = DIRECTION ( 'NONE',  ( 1.000000000000000000, 0.000000000000000000, 0.000000000000000000 ) ) ;
#6672 = CARTESIAN_POINT ( 'NONE',  ( 158.0000000000017337, 42.94087446699998623, 45.00000000000000000 ) ) ;
#6673 = CARTESIAN_POINT ( 'NONE',  ( 222.4999999999996021, 186.4134324495536248, -35.02193266779035952 ) ) ;
#6674 = ORIENTED_EDGE ( 'NONE', *, *, #16437, .F. ) ;
#6675 = CARTESIAN_POINT ( 'NONE',  ( 158.0000000000013927, 73.54324956459154805, -45.00000000000000000 ) ) ;
#6676 = EDGE_LOOP ( 'NONE', ( #18165, #8533, #14269, #7335 ) ) ;
#6677 = DIRECTION ( 'NONE',  ( -1.000000000000000000, 0.000000000000000000, 0.000000000000000000 ) ) ;
#6678 = CARTESIAN_POINT ( 'NONE',  ( -238.3976651326582328, 69.81518760999665574, -5.405651710414773881 ) ) ;
#6679 = DIRECTION ( 'NONE',  ( 1.000000000000000000, 0.000000000000000000, 0.000000000000000000 ) ) ;
#6680 = CARTESIAN_POINT ( 'NONE',  ( 161.2365440327092472, 161.2365440327092472, -45.00000000000000000 ) ) ;
#6681 = CARTESIAN_POINT ( 'NONE',  ( 232.4999999999996305, 133.0668745871126930, -30.86484227207697018 ) ) ;
#6682 = ORIENTED_EDGE ( 'NONE', *, *, #1268, .F. ) ;
#6683 = DIRECTION ( 'NONE',  ( -0.000000000000000000, -0.000000000000000000, -1.000000000000000000 ) ) ;
#6684 = ORIENTED_EDGE ( 'NONE', *, *, #14307, .T. ) ;
#6685 = DIRECTION ( 'NONE',  ( -0.8916010070293483025, -0.4528218681382912281, 0.000000000000000000 ) ) ;
#6686 = ORIENTED_EDGE ( 'NONE', *, *, #15833, .F. ) ;
#6687 = VECTOR ( 'NONE', #26075, 1000.000000000000114 ) ;
#6688 = VERTEX_POINT ( 'NONE', #24782 ) ;
#6689 = PLANE ( 'NONE',  #16802 ) ;
#6690 = EDGE_CURVE ( 'NONE', #19703, #502, #13876, .T. ) ;
#6691 = VERTEX_POINT ( 'NONE', #27066 ) ;
#6692 = CIRCLE ( 'NONE', #3019, 22.49999999999999289 ) ;
#6693 = ORIENTED_EDGE ( 'NONE', *, *, #13132, .T. ) ;
#6694 = CARTESIAN_POINT ( 'NONE',  ( -216.6285193170544687, 139.2238166778980712, 12.99999999956374275 ) ) ;
#6695 = CARTESIAN_POINT ( 'NONE',  ( 94.60831035301521297, 240.0858928317027221, 18.63379520592308936 ) ) ;
#6696 = DIRECTION ( 'NONE',  ( 0.000000000000000000, 0.000000000000000000, -1.000000000000000000 ) ) ;
#6697 = CARTESIAN_POINT ( 'NONE',  ( 209.9999999999999432, 0.000000000000000000, 110.0000000000000284 ) ) ;
#6698 = CARTESIAN_POINT ( 'NONE',  ( 160.9807621135329612, 204.9999999999999147, -138.9999999999999432 ) ) ;
#6699 = CARTESIAN_POINT ( 'NONE',  ( 109.9999999999999432, -120.0000000000001279, 25.00000000000000000 ) ) ;
#6700 = EDGE_CURVE ( 'NONE', #18691, #17779, #11997, .T. ) ;
#6701 = CYLINDRICAL_SURFACE ( 'NONE', #2115, 6.000000000000005329 ) ;
#6702 = DIRECTION ( 'NONE',  ( 0.5773502691896279515, 0.5773502691896280625, 0.5773502691896214012 ) ) ;
#6703 = CARTESIAN_POINT ( 'NONE',  ( 158.0000000000004832, 163.3188748273380213, 45.00000000000000000 ) ) ;
#6704 = PLANE ( 'NONE',  #16669 ) ;
#6705 = VECTOR ( 'NONE', #14676, 1000.000000000000000 ) ;
#6706 = ORIENTED_EDGE ( 'NONE', *, *, #11340, .F. ) ;
#6707 = CARTESIAN_POINT ( 'NONE',  ( -115.3221550338875687, 71.54464929955099706, 83.00000000000001421 ) ) ;
#6708 = LINE ( 'NONE', #4548, #27063 ) ;
#6709 = CARTESIAN_POINT ( 'NONE',  ( 158.0000000000007674, 133.2243747372535267, -45.00000000000000000 ) ) ;
#6710 = CARTESIAN_POINT ( 'NONE',  ( -217.2892621185082760, 109.4029876883478352, 15.00000000000000000 ) ) ;
#6711 = CIRCLE ( 'NONE', #19098, 6.000000000000005329 ) ;
#6712 = VERTEX_POINT ( 'NONE', #1345 ) ;
#6713 = EDGE_CURVE ( 'NONE', #16287, #26306, #18454, .T. ) ;
#6714 = EDGE_CURVE ( 'NONE', #9424, #21781, #5796, .T. ) ;
#6715 = CARTESIAN_POINT ( 'NONE',  ( 158.0000000000014211, 68.52749954957745615, 45.00000000000000000 ) ) ;
#6716 = VERTEX_POINT ( 'NONE', #25062 ) ;
#6717 = CARTESIAN_POINT ( 'NONE',  ( -33.76020577399351907, 129.4009239033509573, -15.57932736426030118 ) ) ;
#6718 = EDGE_LOOP ( 'NONE', ( #9735, #17642, #4204, #10334 ) ) ;
#6719 = ORIENTED_EDGE ( 'NONE', *, *, #12645, .F. ) ;
#6720 = EDGE_LOOP ( 'NONE', ( #20461, #8466, #2321, #21953 ) ) ;
#6721 = EDGE_LOOP ( 'NONE', ( #1698, #7942, #1319, #3066 ) ) ;
#6722 = ORIENTED_EDGE ( 'NONE', *, *, #27605, .F. ) ;
#6723 = CIRCLE ( 'NONE', #15462, 5.999999999999991118 ) ;
#6724 = DIRECTION ( 'NONE',  ( 1.000000000000000000, 0.000000000000000000, 0.000000000000000000 ) ) ;
#6725 = DIRECTION ( 'NONE',  ( -1.541976423090495387E-16, 1.000000000000000000, 0.000000000000000000 ) ) ;
#6726 = DIRECTION ( 'NONE',  ( -0.000000000000000000, -0.000000000000000000, -1.000000000000000000 ) ) ;
#6727 = ADVANCED_FACE ( 'NONE', ( #25606 ), #1066, .F. ) ;
#6728 = CARTESIAN_POINT ( 'NONE',  ( -213.6504899993254298, 58.00877466446878827, 34.94433424773627905 ) ) ;
#6729 = DIRECTION ( 'NONE',  ( 0.000000000000000000, 0.000000000000000000, 1.000000000000000000 ) ) ;
#6730 = DIRECTION ( 'NONE',  ( -0.8916010070296733758, -0.4528218681376511845, 0.000000000000000000 ) ) ;
#6731 = EDGE_CURVE ( 'NONE', #13530, #21087, #8096, .T. ) ;
#6732 = DIRECTION ( 'NONE',  ( -0.8916010070300285362, -0.4528218681369517995, 0.000000000000000000 ) ) ;
#6733 = DIRECTION ( 'NONE',  ( 1.000000000000000000, 0.000000000000000000, 0.000000000000000000 ) ) ;
#6734 = DIRECTION ( 'NONE',  ( -0.8916010070293783896, 0.4528218681382319422, 0.000000000000000000 ) ) ;
#6735 = CARTESIAN_POINT ( 'NONE',  ( -40.40953891503691153, 0.000000000000000000, 100.0000000000000000 ) ) ;
#6736 = FACE_OUTER_BOUND ( 'NONE', #22344, .T. ) ;
#6737 = DIRECTION ( 'NONE',  ( 0.4528218681382909505, 0.8916010070293484135, -0.000000000000000000 ) ) ;
#6738 = DIRECTION ( 'NONE',  ( 0.000000000000000000, 1.000000000000000000, 1.214306433183764966E-16 ) ) ;
#6739 = DIRECTION ( 'NONE',  ( 0.000000000000000000, 0.000000000000000000, 1.000000000000000000 ) ) ;
#6741 = VERTEX_POINT ( 'NONE', #25192 ) ;
#6740 = ORIENTED_EDGE ( 'NONE', *, *, #10198, .T. ) ;
#6742 = CIRCLE ( 'NONE', #20511, 5.999999999999977796 ) ;
#6743 = EDGE_CURVE ( 'NONE', #20893, #5272, #7815, .T. ) ;
#6744 = CARTESIAN_POINT ( 'NONE',  ( -178.9685328442623131, 110.6385515672100581, 29.32315025982155987 ) ) ;
#6745 = AXIS2_PLACEMENT_3D ( 'NONE', #25804, #6130, #14905 ) ;
#6746 = CARTESIAN_POINT ( 'NONE',  ( 158.0000000000001421, 193.4133749174225443, 45.00000000000000000 ) ) ;
#6747 = ORIENTED_EDGE ( 'NONE', *, *, #20444, .F. ) ;
#6748 = ITEM_DEFINED_TRANSFORMATION ( 'NONE', 'NONE', #24418,  #10637 ) ;
#6749 = ORIENTED_EDGE ( 'NONE', *, *, #6986, .F. ) ;
#6750 = ADVANCED_FACE ( 'NONE', ( #21017 ), #5371, .F. ) ;
#6752 = EDGE_CURVE ( 'NONE', #5309, #4946, #24311, .T. ) ;
#6751 = ORIENTED_EDGE ( 'NONE', *, *, #24894, .F. ) ;
#6753 = CARTESIAN_POINT ( 'NONE',  ( 157.4999999999998579, 118.4310621959647563, 45.00000000000000000 ) ) ;
#6754 = DIRECTION ( 'NONE',  ( -1.000000000000000000, 0.000000000000000000, 0.000000000000000000 ) ) ;
#6755 = ORIENTED_EDGE ( 'NONE', *, *, #4388, .T. ) ;
#6756 = EDGE_CURVE ( 'NONE', #28122, #7774, #16581, .T. ) ;
#6757 = CARTESIAN_POINT ( 'NONE',  ( 90.92319367352099846, 112.0484670279005570, -72.65625000014701129 ) ) ;
#6758 = DIRECTION ( 'NONE',  ( 0.000000000000000000, 0.000000000000000000, 1.000000000000000000 ) ) ;
#6759 = ORIENTED_EDGE ( 'NONE', *, *, #17984, .F. ) ;
#6760 = CARTESIAN_POINT ( 'NONE',  ( -223.8831450509237015, 88.82371471167537891, 14.62991863724387542 ) ) ;
#6761 = VECTOR ( 'NONE', #17221, 1000.000000000000000 ) ;
#6762 = LINE ( 'NONE', #4748, #21720 ) ;
#6763 = DIRECTION ( 'NONE',  ( -0.000000000000000000, 1.000000000000000000, -1.387778780781445429E-16 ) ) ;
#6764 = EDGE_CURVE ( 'NONE', #13241, #24120, #16444, .T. ) ;
#6765 = CARTESIAN_POINT ( 'NONE',  ( 159.2479102360155423, 202.3346240999630368, -139.9049692442122534 ) ) ;
#6766 = ORIENTED_EDGE ( 'NONE', *, *, #6654, .F. ) ;
#6767 = DIRECTION ( 'NONE',  ( -0.000000000000000000, -0.000000000000000000, 1.000000000000000000 ) ) ;
#6768 = CARTESIAN_POINT ( 'NONE',  ( 124.3660254037843771, 240.4185842870417105, 45.00000000000000000 ) ) ;
#6769 = CARTESIAN_POINT ( 'NONE',  ( 158.0000000000000853, 198.9369999399436892, 45.00000000000000000 ) ) ;
#6770 = CARTESIAN_POINT ( 'NONE',  ( 157.9999999999997158, 263.6338751276190351, 45.00000000000000000 ) ) ;
#6771 = EDGE_LOOP ( 'NONE', ( #12390, #23397, #20599, #11105 ) ) ;
#6772 = LINE ( 'NONE', #26028, #2733 ) ;
#6773 = AXIS2_PLACEMENT_3D ( 'NONE', #5006, #5296, #13798 ) ;
#6774 = B_SPLINE_CURVE_WITH_KNOTS ( 'NONE', 3,
 ( #23254, #16789, #16925, #12348, #22971, #18657, #20951, #3557, #23114, #18797 ),
 .UNSPECIFIED., .F., .F.,
 ( 4, 2, 2, 2, 4 ),
 ( 0.000000000000000000, 0.003185215742235096223, 0.006370431484470192446, 0.009555647226705288669, 0.01274086296894038489 ),
 .UNSPECIFIED. ) ;
#6775 = CARTESIAN_POINT ( 'NONE',  ( -210.0000000000000568, -157.0000000000000284, 90.00000000000002842 ) ) ;
#6776 = CIRCLE ( 'NONE', #5412, 5.999999999999977796 ) ;
#6777 = DIRECTION ( 'NONE',  ( 1.000000000000000000, 0.000000000000000000, 0.000000000000000000 ) ) ;
#6778 = ORIENTED_EDGE ( 'NONE', *, *, #10204, .F. ) ;
#6779 =( NAMED_UNIT ( * ) SI_UNIT ( $, .STERADIAN. ) SOLID_ANGLE_UNIT ( ) );
#6780 = ORIENTED_EDGE ( 'NONE', *, *, #16275, .F. ) ;
#6781 = EDGE_CURVE ( 'NONE', #1313, #18620, #22902, .T. ) ;
#6782 = ADVANCED_FACE ( 'NONE', ( #25336 ), #7542, .F. ) ;
#6783 = DIRECTION ( 'NONE',  ( 0.4528218681382713551, 0.8916010070293584056, -0.000000000000000000 ) ) ;
#6784 = ADVANCED_FACE ( 'NONE', ( #3211 ), #3068, .F. ) ;
#6785 = DIRECTION ( 'NONE',  ( 0.000000000000000000, 0.000000000000000000, -1.000000000000000000 ) ) ;
#6786 = ORIENTED_EDGE ( 'NONE', *, *, #3300, .T. ) ;
#6787 = ORIENTED_EDGE ( 'NONE', *, *, #25525, .T. ) ;
#6788 = CARTESIAN_POINT ( 'NONE',  ( 2.399999999999999911, 1.249999999999999556, -8.000000000000000000 ) ) ;
#6789 = DIRECTION ( 'NONE',  ( -1.850371707708594316E-16, 1.000000000000000000, -0.000000000000000000 ) ) ;
#6790 = VECTOR ( 'NONE', #20646, 1000.000000000000000 ) ;
#6791 = VERTEX_POINT ( 'NONE', #27337 ) ;
#6792 = ORIENTED_EDGE ( 'NONE', *, *, #22342, .F. ) ;
#6793 = LINE ( 'NONE', #2334, #14842 ) ;
#6794 = VECTOR ( 'NONE', #5542, 999.9999999999998863 ) ;
#6795 = VECTOR ( 'NONE', #17128, 1000.000000000000114 ) ;
#6796 = LINE ( 'NONE', #23908, #18604 ) ;
#6797 = LINE ( 'NONE', #2920, #15361 ) ;
#6798 = PLANE ( 'NONE',  #11744 ) ;
#6799 = CARTESIAN_POINT ( 'NONE',  ( -56.02075117275366978, 110.3042093914830559, 45.00000000000000000 ) ) ;
#6800 = DIRECTION ( 'NONE',  ( 1.000000000000000000, 0.000000000000000000, 0.000000000000000000 ) ) ;
#6801 = CARTESIAN_POINT ( 'NONE',  ( -160.0000000000000284, 139.9999999999999432, -15.00000000000000000 ) ) ;
#6802 = ORIENTED_EDGE ( 'NONE', *, *, #23855, .T. ) ;
#6803 = DIRECTION ( 'NONE',  ( 0.000000000000000000, 1.387778780781445182E-16, -1.000000000000000000 ) ) ;
#6804 = LINE ( 'NONE', #4228, #20268 ) ;
#6805 = CARTESIAN_POINT ( 'NONE',  ( 187.4999999999996305, 288.9665627064425166, 45.00000000000000000 ) ) ;
#6806 = DIRECTION ( 'NONE',  ( -0.000000000000000000, -1.000000000000000000, -0.000000000000000000 ) ) ;
#6807 = VERTEX_POINT ( 'NONE', #23042 ) ;
#6808 = CARTESIAN_POINT ( 'NONE',  ( -227.3759666274727351, 63.27997354833446764, 7.997465051287307780 ) ) ;
#6809 = EDGE_LOOP ( 'NONE', ( #8133, #13894, #856, #5510 ) ) ;
#6810 = VECTOR ( 'NONE', #5824, 1000.000000000000000 ) ;
#6811 = DIRECTION ( 'NONE',  ( 1.000000000000000000, 0.000000000000000000, 0.000000000000000000 ) ) ;
#6812 = DIRECTION ( 'NONE',  ( -0.8916010070293584056, 0.4528218681382713551, 0.000000000000000000 ) ) ;
#6813 = CARTESIAN_POINT ( 'NONE',  ( 140.8071701735416354, 249.4326844987137974, -143.4408232581956213 ) ) ;
#6814 = ORIENTED_EDGE ( 'NONE', *, *, #19780, .T. ) ;
#6815 = CARTESIAN_POINT ( 'NONE',  ( 113.4999999999998863, 220.0000000000000284, -100.0000000000000142 ) ) ;
#6816 = DIRECTION ( 'NONE',  ( -0.000000000000000000, -0.000000000000000000, -1.000000000000000000 ) ) ;
#6817 = ORIENTED_EDGE ( 'NONE', *, *, #13917, .F. ) ;
#6818 = ADVANCED_FACE ( 'NONE', ( #23185 ), #3353, .T. ) ;
#6819 = AXIS2_PLACEMENT_3D ( 'NONE', #20023, #4931, #2930 ) ;
#6820 = CARTESIAN_POINT ( 'NONE',  ( -219.5796349382799519, 71.26926967086903630, 22.06234792876918149 ) ) ;
#6821 = EDGE_LOOP ( 'NONE', ( #23477, #17707, #8604, #27408 ) ) ;
#6822 = EDGE_CURVE ( 'NONE', #21449, #18495, #19735, .T. ) ;
#6823 = CARTESIAN_POINT ( 'NONE',  ( -272.9248965604650721, -165.1577306887913892, 108.4106317744307262 ) ) ;
#6824 = AXIS2_PLACEMENT_3D ( 'NONE', #20303, #16293, #5357 ) ;
#6825 = ORIENTED_EDGE ( 'NONE', *, *, #21387, .F. ) ;
#6826 = ORIENTED_EDGE ( 'NONE', *, *, #23299, .T. ) ;
#6827 = DIRECTION ( 'NONE',  ( 0.8916010070294800860, -0.4528218681380314359, 0.000000000000000000 ) ) ;
#6828 = EDGE_LOOP ( 'NONE', ( #11383, #5489, #16440, #23769 ) ) ;
#6829 = AXIS2_PLACEMENT_3D ( 'NONE', #22468, #18304, #24768 ) ;
#6830 = ORIENTED_EDGE ( 'NONE', *, *, #20422, .T. ) ;
#6831 = ORIENTED_EDGE ( 'NONE', *, *, #11017, .F. ) ;
#6832 = LINE ( 'NONE', #12893, #13680 ) ;
#6833 = CARTESIAN_POINT ( 'NONE',  ( 88.05061285011872485, 239.8951213613607365, 16.09479252966118068 ) ) ;
#6834 = VECTOR ( 'NONE', #7811, 1000.000000000000000 ) ;
#6835 = CARTESIAN_POINT ( 'NONE',  ( -273.6211430000234373, -91.18033988749901653, -14.64217782292691261 ) ) ;
#6836 = AXIS2_PLACEMENT_3D ( 'NONE', #15190, #28363, #8575 ) ;
#6837 = DIRECTION ( 'NONE',  ( -0.000000000000000000, -0.000000000000000000, 1.000000000000000000 ) ) ;
#6838 = DIRECTION ( 'NONE',  ( -0.000000000000000000, -0.000000000000000000, -1.000000000000000000 ) ) ;
#6839 = VECTOR ( 'NONE', #18939, 1000.000000000000114 ) ;
#6840 = CARTESIAN_POINT ( 'NONE',  ( 134.1167547769962596, -7.205103435269982093, 45.00000000000000000 ) ) ;
#6841 = CYLINDRICAL_SURFACE ( 'NONE', #1010, 43.76444293738735070 ) ;
#6842 = CARTESIAN_POINT ( 'NONE',  ( -17.24491960465746132, 75.97823757117562593, 95.00000000000000000 ) ) ;
#6843 = CARTESIAN_POINT ( 'NONE',  ( 158.0000000000000000, 208.4606249624626457, 45.00000000000000000 ) ) ;
#6844 = DIRECTION ( 'NONE',  ( 0.000000000000000000, 0.000000000000000000, -1.000000000000000000 ) ) ;
#6845 = LINE ( 'NONE', #26660, #20560 ) ;
#6846 = DIRECTION ( 'NONE',  ( 0.000000000000000000, 0.000000000000000000, -1.000000000000000000 ) ) ;
#6847 = ORIENTED_EDGE ( 'NONE', *, *, #7733, .F. ) ;
#6848 = FACE_OUTER_BOUND ( 'NONE', #23215, .T. ) ;
#6849 = AXIS2_PLACEMENT_3D ( 'NONE', #12652, #21531, #12928 ) ;
#6850 = EDGE_CURVE ( 'NONE', #13481, #23690, #4596, .T. ) ;
#6851 = CARTESIAN_POINT ( 'NONE',  ( 157.4999999999998579, 153.5413123010633853, 45.00000000000000000 ) ) ;
#6852 = LINE ( 'NONE', #5124, #6632 ) ;
#6853 = CARTESIAN_POINT ( 'NONE',  ( -210.0000000000000284, 59.99999999999994316, 17.29233506344265336 ) ) ;
#6854 = ORIENTED_EDGE ( 'NONE', *, *, #9877, .T. ) ;
#6855 = AXIS2_PLACEMENT_3D ( 'NONE', #9796, #14111, #7361 ) ;
#6856 = CARTESIAN_POINT ( 'NONE',  ( 109.7119445822053194, 256.4759837302104302, -40.72317850545796603 ) ) ;
#6857 = VERTEX_POINT ( 'NONE', #12424 ) ;
#6858 = ADVANCED_FACE ( 'NONE', ( #14857 ), #12864, .T. ) ;
#6859 = CARTESIAN_POINT ( 'NONE',  ( 158.0000000000009948, 108.6534996696901345, -45.00000000000000000 ) ) ;
#6860 = VERTEX_POINT ( 'NONE', #25893 ) ;
#6861 =( GEOMETRIC_REPRESENTATION_CONTEXT ( 3 ) GLOBAL_UNCERTAINTY_ASSIGNED_CONTEXT ( ( #8892 ) ) GLOBAL_UNIT_ASSIGNED_CONTEXT ( ( #10431, #1099, #18624 ) ) REPRESENTATION_CONTEXT ( 'NONE', 'WORKASPACE' ) );
#6862 = ORIENTED_EDGE ( 'NONE', *, *, #17460, .T. ) ;
#6863 = VECTOR ( 'NONE', #12876, 1000.000000000000000 ) ;
#6864 = EDGE_CURVE ( 'NONE', #9172, #4836, #6216, .T. ) ;
#6865 = ORIENTED_EDGE ( 'NONE', *, *, #6405, .F. ) ;
#6866 = ORIENTED_EDGE ( 'NONE', *, *, #22705, .T. ) ;
#6867 = EDGE_LOOP ( 'NONE', ( #16279, #13488, #7411, #17852 ) ) ;
#6868 = ORIENTED_EDGE ( 'NONE', *, *, #18826, .F. ) ;
#6869 = CARTESIAN_POINT ( 'NONE',  ( -112.3221550338875687, 22.24192588826928585, 80.00000000000001421 ) ) ;
#6870 = PLANE ( 'NONE',  #592 ) ;
#6871 = AXIS2_PLACEMENT_3D ( 'NONE', #2552, #17500, #11339 ) ;
#6872 = DIRECTION ( 'NONE',  ( -0.000000000000000000, 0.000000000000000000, -1.000000000000000000 ) ) ;
#6873 = CARTESIAN_POINT ( 'NONE',  ( 232.4999999999996305, 194.4107529906318064, 288.0938197134494203 ) ) ;
#6874 = ADVANCED_FACE ( 'NONE', ( #21586 ), #25746, .F. ) ;
#6875 = CARTESIAN_POINT ( 'NONE',  ( -222.1142713347912263, 61.47487629660645325, 10.02481564199105613 ) ) ;
#6876 = PLANE ( 'NONE',  #26390 ) ;
#6877 = CARTESIAN_POINT ( 'NONE',  ( 40.99999999999999289, 0.000000000000000000, 5.000000000000000000 ) ) ;
#6878 = CIRCLE ( 'NONE', #21556, 6.000000000000005329 ) ;
#6879 = PLANE ( 'NONE',  #14500 ) ;
#6880 = CARTESIAN_POINT ( 'NONE',  ( -190.0000000000000284, -2.775557561562891982E-14, 98.28427124746191623 ) ) ;
#6881 = DIRECTION ( 'NONE',  ( 0.4528218681376312005, 0.8916010070296835899, -0.000000000000000000 ) ) ;
#6882 = AXIS2_PLACEMENT_3D ( 'NONE', #1896, #2042, #19291 ) ;
#6883 = EDGE_CURVE ( 'NONE', #2675, #25971, #17901, .T. ) ;
#6884 = CARTESIAN_POINT ( 'NONE',  ( -7.230610758732472831, 132.9655077820579265, 15.80094727182378023 ) ) ;
#6885 = LINE ( 'NONE', #8622, #899 ) ;
#6886 = LINE ( 'NONE', #4724, #6018 ) ;
#6887 = DIRECTION ( 'NONE',  ( 1.000000000000000000, 0.000000000000000000, 0.000000000000000000 ) ) ;
#6889 = ORIENTED_EDGE ( 'NONE', *, *, #28214, .T. ) ;
#6888 = EDGE_LOOP ( 'NONE', ( #24221, #12671, #19443, #20155 ) ) ;
#6890 = CARTESIAN_POINT ( 'NONE',  ( -214.7362006204176339, 86.61744048289359910, -21.86430821152871928 ) ) ;
#6891 = CARTESIAN_POINT ( 'NONE',  ( 157.4999999999994884, 211.2224374737238577, -45.00000000000000000 ) ) ;
#6892 = CARTESIAN_POINT ( 'NONE',  ( -207.2804935778247568, 89.57475743267312396, -27.31082310662946000 ) ) ;
#6893 = ORIENTED_EDGE ( 'NONE', *, *, #12211, .F. ) ;
#6894 = EDGE_LOOP ( 'NONE', ( #10162, #3199, #25412, #6040 ) ) ;
#6895 = VERTEX_POINT ( 'NONE', #14994 ) ;
#6896 = EDGE_CURVE ( 'NONE', #3365, #23798, #10393, .T. ) ;
#6897 = CARTESIAN_POINT ( 'NONE',  ( 179.9999999999999147, 330.0000000000000000, 100.0000000000000142 ) ) ;
#6898 = AXIS2_PLACEMENT_3D ( 'NONE', #23629, #3939, #6240 ) ;
#6899 = EDGE_CURVE ( 'NONE', #15077, #2290, #13800, .T. ) ;
#6900 = FACE_OUTER_BOUND ( 'NONE', #23005, .T. ) ;
#6901 = ORIENTED_EDGE ( 'NONE', *, *, #276, .F. ) ;
#6902 = ORIENTED_EDGE ( 'NONE', *, *, #2440, .F. ) ;
#6903 = CARTESIAN_POINT ( 'NONE',  ( 109.9999999999999005, 3.816391647148972452E-14, 100.0000000000000142 ) ) ;
#6904 = DIRECTION ( 'NONE',  ( -0.000000000000000000, -0.000000000000000000, -1.000000000000000000 ) ) ;
#6905 = ORIENTED_EDGE ( 'NONE', *, *, #2402, .F. ) ;
#6906 = CARTESIAN_POINT ( 'NONE',  ( -203.7080335011695809, 92.59420371806315586, 28.49755056600432823 ) ) ;
#6907 = DIRECTION ( 'NONE',  ( 1.000000000000000000, -0.000000000000000000, -0.000000000000000000 ) ) ;
#6908 = EDGE_CURVE ( 'NONE', #6688, #4667, #6436, .T. ) ;
#6909 = EDGE_CURVE ( 'NONE', #11282, #7826, #19147, .T. ) ;
#6910 = LINE ( 'NONE', #4750, #16728 ) ;
#6911 = FACE_OUTER_BOUND ( 'NONE', #23459, .T. ) ;
#6912 = CARTESIAN_POINT ( 'NONE',  ( -198.1081924558745584, 61.84288891412396083, -30.88603804298208644 ) ) ;
#6913 = VERTEX_POINT ( 'NONE', #23890 ) ;
#6914 = AXIS2_PLACEMENT_3D ( 'NONE', #3617, #16846, #14693 ) ;
#6915 = LINE ( 'NONE', #22722, #21044 ) ;
#6916 = EDGE_CURVE ( 'NONE', #5026, #26072, #21441, .T. ) ;
#6917 = CARTESIAN_POINT ( 'NONE',  ( 294.9233831825460470, 127.6681916698403398, -145.0000000000000000 ) ) ;
#6918 = DIRECTION ( 'NONE',  ( -0.000000000000000000, -0.000000000000000000, -1.000000000000000000 ) ) ;
#6919 = DIRECTION ( 'NONE',  ( -0.000000000000000000, 0.000000000000000000, 1.000000000000000000 ) ) ;
#6920 = EDGE_LOOP ( 'NONE', ( #8074, #22296, #2182, #5332, #8101, #3077 ) ) ;
#6921 = FACE_OUTER_BOUND ( 'NONE', #12712, .T. ) ;
#6922 = VECTOR ( 'NONE', #16263, 1000.000000000000000 ) ;
#6923 = DIRECTION ( 'NONE',  ( -0.7071067811865435759, 0.000000000000000000, 0.7071067811865514585 ) ) ;
#6924 = LINE ( 'NONE', #24308, #13090 ) ;
#6925 = VERTEX_POINT ( 'NONE', #8235 ) ;
#6926 = ORIENTED_EDGE ( 'NONE', *, *, #4183, .T. ) ;
#6927 = CARTESIAN_POINT ( 'NONE',  ( -295.0000000000001705, -157.0000000000000284, -59.99999999999986500 ) ) ;
#6928 = CARTESIAN_POINT ( 'NONE',  ( -160.0000000000000284, 59.99999999999994316, 98.28427124746191623 ) ) ;
#6929 = ORIENTED_EDGE ( 'NONE', *, *, #8957, .F. ) ;
#6930 = EDGE_LOOP ( 'NONE', ( #12812, #28287, #6463, #21741 ) ) ;
#6931 = DIRECTION ( 'NONE',  ( -1.000000000000000000, -0.000000000000000000, 0.000000000000000000 ) ) ;
#6932 = AXIS2_PLACEMENT_3D ( 'NONE', #1686, #21799, #10454 ) ;
#6933 = CARTESIAN_POINT ( 'NONE',  ( 157.4999999999998579, 188.6515624061619576, 45.00000000000000000 ) ) ;
#6934 = ORIENTED_EDGE ( 'NONE', *, *, #13626, .F. ) ;
#6935 = ORIENTED_EDGE ( 'NONE', *, *, #15210, .F. ) ;
#6936 = DIRECTION ( 'NONE',  ( -0.4528218681382693567, 0.8916010070293595158, 0.000000000000000000 ) ) ;
#6937 = AXIS2_PLACEMENT_3D ( 'NONE', #23083, #16205, #25094 ) ;
#6938 = DIRECTION ( 'NONE',  ( -1.000000000000000000, 7.930164461608265370E-16, 0.000000000000000000 ) ) ;
#6939 = DIRECTION ( 'NONE',  ( 0.4528218681378916588, 0.8916010070295512513, -0.000000000000000000 ) ) ;
#6940 = CARTESIAN_POINT ( 'NONE',  ( -8.342823007631203325, 132.5495086141303318, -15.90323448772006643 ) ) ;
#6941 = EDGE_CURVE ( 'NONE', #13442, #25647, #10676, .T. ) ;
#6942 = DIRECTION ( 'NONE',  ( 1.000000000000000000, 0.000000000000000000, 0.000000000000000000 ) ) ;
#6943 = EDGE_CURVE ( 'NONE', #17824, #15830, #4143, .T. ) ;
#6944 = CARTESIAN_POINT ( 'NONE',  ( -210.0000000000000284, 59.99999999999993605, -17.29233506344264626 ) ) ;
#6945 = ORIENTED_EDGE ( 'NONE', *, *, #956, .F. ) ;
#6946 = CARTESIAN_POINT ( 'NONE',  ( 134.9999999999998579, 220.0000000000000284, 99.00000000000001421 ) ) ;
#6947 = DIRECTION ( 'NONE',  ( 0.8916010070293383105, -0.4528218681383106015, 0.000000000000000000 ) ) ;
#6948 = DIRECTION ( 'NONE',  ( 1.000000000000000000, -0.000000000000000000, -0.000000000000000000 ) ) ;
#6949 = DIRECTION ( 'NONE',  ( 1.000000000000000000, 0.000000000000000000, 0.000000000000000000 ) ) ;
#6950 = ORIENTED_EDGE ( 'NONE', *, *, #11254, .F. ) ;
#6951 = CARTESIAN_POINT ( 'NONE',  ( 158.0000000000007105, 136.2401247522676044, -45.00000000000000000 ) ) ;
#6952 = ORIENTED_EDGE ( 'NONE', *, *, #3439, .F. ) ;
#6953 = VECTOR ( 'NONE', #26311, 1000.000000000000000 ) ;
#6954 = CARTESIAN_POINT ( 'NONE',  ( 134.9999999999998579, 220.0000000000000284, -105.0000000000000284 ) ) ;
#6955 = LINE ( 'NONE', #26787, #9664 ) ;
#6956 = CARTESIAN_POINT ( 'NONE',  ( 140.9998454966672625, 249.3939084512563511, -145.3948054049556617 ) ) ;
#6957 = ORIENTED_EDGE ( 'NONE', *, *, #23570, .T. ) ;
#6958 =( LENGTH_UNIT ( ) NAMED_UNIT ( * ) SI_UNIT ( .MILLI., .METRE. ) );
#6959 = LINE ( 'NONE', #4803, #558 ) ;
#6960 = VECTOR ( 'NONE', #6083, 1000.000000000000114 ) ;
#6961 = ORIENTED_EDGE ( 'NONE', *, *, #27696, .T. ) ;
#6962 = TOROIDAL_SURFACE ( 'NONE', #19330, 16.91094714394370158, 6.204828372381208546 ) ;
#6963 = CYLINDRICAL_SURFACE ( 'NONE', #2886, 10.00000000000000888 ) ;
#6964 = VERTEX_POINT ( 'NONE', #7764 ) ;
#6965 = CARTESIAN_POINT ( 'NONE',  ( -274.6324364865060943, -170.0364449491623589, -102.6462360633263984 ) ) ;
#6966 = ORIENTED_EDGE ( 'NONE', *, *, #445, .F. ) ;
#6967 = EDGE_LOOP ( 'NONE', ( #10705, #9354, #17530, #10365 ) ) ;
#6968 = DIRECTION ( 'NONE',  ( -0.000000000000000000, 0.000000000000000000, -1.000000000000000000 ) ) ;
#6969 = EDGE_LOOP ( 'NONE', ( #17569, #7993 ) ) ;
#6970 = EDGE_CURVE ( 'NONE', #16435, #2005, #11947, .T. ) ;
#6971 = ORIENTED_EDGE ( 'NONE', *, *, #18909, .T. ) ;
#6972 = ORIENTED_EDGE ( 'NONE', *, *, #25716, .T. ) ;
#6973 = CARTESIAN_POINT ( 'NONE',  ( 100.2919976486527247, 242.8371140006016162, 14.10862752716273150 ) ) ;
#6974 = AXIS2_PLACEMENT_3D ( 'NONE', #25852, #19251, #1159 ) ;
#6975 = DIRECTION ( 'NONE',  ( -0.000000000000000000, -0.000000000000000000, -1.000000000000000000 ) ) ;
#6976 = EDGE_CURVE ( 'NONE', #5248, #18824, #27969, .T. ) ;
#6977 = DIRECTION ( 'NONE',  ( 1.321694076934710155E-16, -1.000000000000000000, 0.000000000000000000 ) ) ;
#6978 = AXIS2_PLACEMENT_3D ( 'NONE', #26508, #4536, #22507 ) ;
#6979 =( GEOMETRIC_REPRESENTATION_CONTEXT ( 3 ) GLOBAL_UNCERTAINTY_ASSIGNED_CONTEXT ( ( #13789 ) ) GLOBAL_UNIT_ASSIGNED_CONTEXT ( ( #15284, #8380, #22012 ) ) REPRESENTATION_CONTEXT ( 'NONE', 'WORKASPACE' ) );
#6980 = ADVANCED_FACE ( 'NONE', ( #20686 ), #25556, .F. ) ;
#6981 = AXIS2_PLACEMENT_3D ( 'NONE', #17031, #17177, #21340 ) ;
#6982 = ADVANCED_FACE ( 'NONE', ( #7898, #1291, #5601, #12089, #5740, #3440 ), #3718, .F. ) ;
#6983 = LINE ( 'NONE', #17471, #9183 ) ;
#6984 = DIRECTION ( 'NONE',  ( 1.000000000000000000, 1.153591111524576718E-14, 0.000000000000000000 ) ) ;
#6985 = FACE_OUTER_BOUND ( 'NONE', #15560, .T. ) ;
#6986 = EDGE_CURVE ( 'NONE', #22985, #10405, #1152, .T. ) ;
#6987 = CARTESIAN_POINT ( 'NONE',  ( 2.399999999999999911, -1.249999999999999112, -7.582700855991164168 ) ) ;
#6988 = PLANE ( 'NONE',  #19056 ) ;
#6989 = FACE_OUTER_BOUND ( 'NONE', #26027, .T. ) ;
#6990 = LINE ( 'NONE', #24948, #13236 ) ;
#6991 = DIRECTION ( 'NONE',  ( 1.000000000000000000, -0.000000000000000000, -0.000000000000000000 ) ) ;
#6992 = ORIENTED_EDGE ( 'NONE', *, *, #5988, .T. ) ;
#6993 = CARTESIAN_POINT ( 'NONE',  ( 158.0000000000016200, 50.97237449702815582, -45.00000000000000000 ) ) ;
#6994 = DIRECTION ( 'NONE',  ( -0.000000000000000000, 0.000000000000000000, 1.000000000000000000 ) ) ;
#6995 = CARTESIAN_POINT ( 'NONE',  ( 157.9999999999997726, 244.0787500750700474, 45.00000000000000000 ) ) ;
#6996 = CARTESIAN_POINT ( 'NONE',  ( 108.8246248949738373, 205.3409232530312636, -139.0095862629494547 ) ) ;
#6997 = ORIENTED_EDGE ( 'NONE', *, *, #22454, .T. ) ;
#6998 = VECTOR ( 'NONE', #1456, 1000.000000000000000 ) ;
#6999 = VECTOR ( 'NONE', #7610, 1000.000000000000000 ) ;
#7000 = CARTESIAN_POINT ( 'NONE',  ( -210.0000000000000568, -152.0000000000000284, 95.00000000000004263 ) ) ;
#7001 = ORIENTED_EDGE ( 'NONE', *, *, #10419, .T. ) ;
#7002 = CARTESIAN_POINT ( 'NONE',  ( -236.8177751472017007, 82.33896643611703325, -5.000000000000002665 ) ) ;
#7003 = ORIENTED_EDGE ( 'NONE', *, *, #11073, .T. ) ;
#7004 = VECTOR ( 'NONE', #8900, 1000.000000000000114 ) ;
#7005 = CARTESIAN_POINT ( 'NONE',  ( 3.660298066448477439, -2.383854334960948229, -45.00000000000000000 ) ) ;
#7006 = ORIENTED_EDGE ( 'NONE', *, *, #19925, .F. ) ;
#7007 = B_SPLINE_CURVE_WITH_KNOTS ( 'NONE', 3,
 ( #19081, #21376, #21233, #1692, #12914, #21660, #27966, #1972, #6432, #10752, #23964, #27686, #19508, #26104, #14635, #1556, #3700, #28253, #15211, #4276, #21091, #16791, #5861, #18940, #8021, #11323, #398, #9304, #24241, #24672, #13197, #17485, #256, #22085, #108, #26521, #11033, #15354, #4550, #11471, #7145, #6996, #2390, #13061 ),
 .UNSPECIFIED., .F., .F.,
 ( 4, 2, 2, 2, 2, 2, 2, 2, 2, 2, 2, 2, 2, 2, 2, 2, 2, 2, 2, 2, 2, 4 ),
 ( 3.103167691559091397E-17, 0.001175389346958652555, 0.001763084020437963436, 0.002350778693917274318, 0.003526168040875896081, 0.004701557387834517411, 0.005876946734793139608, 0.007052336081751760938, 0.007640030755231059893, 0.008227725428710357114, 0.009403114775668859615, 0.01057850412262736385, 0.01175389346958586462, 0.01234158814306509158, 0.01292928281654431508, 0.01410467216350273084, 0.01528006151046114661, 0.01586775618394034582, 0.01645545085741954502, 0.01763084020437794691, 0.01821853487785714959, 0.01880622955133634880 ),
 .UNSPECIFIED. ) ;
#7008 = ORIENTED_EDGE ( 'NONE', *, *, #23480, .F. ) ;
#7009 = VERTEX_POINT ( 'NONE', #10061 ) ;
#7010 = VERTEX_POINT ( 'NONE', #25701 ) ;
#7011 = ORIENTED_EDGE ( 'NONE', *, *, #9233, .F. ) ;
#7012 = CARTESIAN_POINT ( 'NONE',  ( -175.0000000000000000, -170.0000000000001705, 70.00000000000001421 ) ) ;
#7013 = CARTESIAN_POINT ( 'NONE',  ( 158.0000000000009663, 115.6692496847042264, 45.00000000000000000 ) ) ;
#7014 = EDGE_CURVE ( 'NONE', #2828, #10760, #6023, .T. ) ;
#7015 = EDGE_CURVE ( 'NONE', #24201, #16772, #27288, .T. ) ;
#7016 = PLANE ( 'NONE',  #2264 ) ;
#7017 = CARTESIAN_POINT ( 'NONE',  ( -33.73603230484052773, 129.3982133951581091, 15.58051746129034676 ) ) ;
#7018 = VECTOR ( 'NONE', #15439, 1000.000000000000114 ) ;
#7019 = CARTESIAN_POINT ( 'NONE',  ( -225.5243807178691213, 62.25611586199291025, 19.08347035850884410 ) ) ;
#7020 = CARTESIAN_POINT ( 'NONE',  ( 158.0000000000003979, 170.8424998498591663, 45.00000000000000000 ) ) ;
#7021 = PLANE ( 'NONE',  #1187 ) ;
#7022 = CIRCLE ( 'NONE', #11641, 60.90601976618767566 ) ;
#7023 = ADVANCED_FACE ( 'NONE', ( #25281 ), #25139, .F. ) ;
#7024 = LINE ( 'NONE', #17942, #15425 ) ;
#7025 = LINE ( 'NONE', #13219, #2975 ) ;
#7026 = VECTOR ( 'NONE', #15775, 1000.000000000000000 ) ;
#7027 = DIRECTION ( 'NONE',  ( -1.000000000000000000, 0.000000000000000000, 0.000000000000000000 ) ) ;
#7028 = FACE_OUTER_BOUND ( 'NONE', #1628, .T. ) ;
#7029 = FACE_OUTER_BOUND ( 'NONE', #28154, .T. ) ;
#7030 = CIRCLE ( 'NONE', #3349, 4.999999999999992895 ) ;
#7031 = EDGE_CURVE ( 'NONE', #1602, #21761, #5457, .T. ) ;
#7032 = CARTESIAN_POINT ( 'NONE',  ( -1.259556330921223433, 135.5648644267808436, 13.59427901309335596 ) ) ;
#7033 = DIRECTION ( 'NONE',  ( -1.541976423090495387E-16, 1.000000000000000000, 0.000000000000000000 ) ) ;
#7034 = CARTESIAN_POINT ( 'NONE',  ( 158.0000000000004832, 161.3188748273380213, -45.00000000000000000 ) ) ;
#7035 = DIRECTION ( 'NONE',  ( -0.4999999999999985012, -0.8660254037844394848, 0.000000000000000000 ) ) ;
#7037 = VERTEX_POINT ( 'NONE', #18815 ) ;
#7036 = ORIENTED_EDGE ( 'NONE', *, *, #7185, .T. ) ;
#7038 = CARTESIAN_POINT ( 'NONE',  ( -205.9966200546697905, 90.40127925949050791, -28.21257754844605969 ) ) ;
#7039 = CARTESIAN_POINT ( 'NONE',  ( 133.9999999999998295, 242.9999999999997158, -45.00000000000000000 ) ) ;
#7040 = CARTESIAN_POINT ( 'NONE',  ( 150.5563491861040575, 203.0294372515228929, -45.00000000000000000 ) ) ;
#7041 = ORIENTED_EDGE ( 'NONE', *, *, #7857, .F. ) ;
#7042 = ORIENTED_EDGE ( 'NONE', *, *, #22159, .F. ) ;
#7043 = VECTOR ( 'NONE', #19239, 1000.000000000000000 ) ;
#7044 = VERTEX_POINT ( 'NONE', #3294 ) ;
#7045 = AXIS2_PLACEMENT_3D ( 'NONE', #2056, #26460, #6655 ) ;
#7046 = CARTESIAN_POINT ( 'NONE',  ( 232.4999999999996305, 83.06687458711267880, -30.83984227207693607 ) ) ;
#7047 = CARTESIAN_POINT ( 'NONE',  ( -155.6312558209752979, 121.5918491723093524, 21.28780381422281920 ) ) ;
#7048 = EDGE_LOOP ( 'NONE', ( #10122, #5474, #10610, #10549 ) ) ;
#7049 = AXIS2_PLACEMENT_3D ( 'NONE', #14285, #16160, #27609 ) ;
#7050 = ORIENTED_EDGE ( 'NONE', *, *, #9551, .F. ) ;
#7051 = DIRECTION ( 'NONE',  ( -0.000000000000000000, -0.000000000000000000, -1.000000000000000000 ) ) ;
#7052 = EDGE_CURVE ( 'NONE', #9545, #15146, #18676, .T. ) ;
#7053 = CARTESIAN_POINT ( 'NONE',  ( 5.999999999999998224, 9.797174393178825657E-16, 8.000000000000000000 ) ) ;
#7054 = EDGE_LOOP ( 'NONE', ( #22037, #8879, #3959, #23191 ) ) ;
#7055 = CARTESIAN_POINT ( 'NONE',  ( 1.982541115402066017E-14, -150.0000000000000568, -99.99999999999995737 ) ) ;
#7056 = CARTESIAN_POINT ( 'NONE',  ( 104.2819297219271562, 239.9331382545718441, -27.31288972538037996 ) ) ;
#7057 = DIRECTION ( 'NONE',  ( -0.000000000000000000, 1.000000000000000000, -0.000000000000000000 ) ) ;
#7058 = DIRECTION ( 'NONE',  ( -0.000000000000000000, -0.000000000000000000, -1.000000000000000000 ) ) ;
#7059 = CARTESIAN_POINT ( 'NONE',  ( -213.7039558558103352, 55.82027786946292025, -42.47917487896670963 ) ) ;
#7060 = VECTOR ( 'NONE', #17293, 1000.000000000000000 ) ;
#7061 = ORIENTED_EDGE ( 'NONE', *, *, #24007, .T. ) ;
#7062 = EDGE_CURVE ( 'NONE', #17988, #21244, #23274, .T. ) ;
#7063 = EDGE_CURVE ( 'NONE', #17486, #25274, #22035, .T. ) ;
#7064 = DIRECTION ( 'NONE',  ( 0.4528218681378310406, 0.8916010070295820045, -0.000000000000000000 ) ) ;
#7065 = CARTESIAN_POINT ( 'NONE',  ( -224.3418196798764086, 136.6081117166938839, -14.97424725141357094 ) ) ;
#7066 = FACE_OUTER_BOUND ( 'NONE', #21655, .T. ) ;
#7067 = CARTESIAN_POINT ( 'NONE',  ( 176.1454027868280434, 57.48855481560072889, 45.00000000000000000 ) ) ;
#7068 = ORIENTED_EDGE ( 'NONE', *, *, #19112, .F. ) ;
#7069 = LINE ( 'NONE', #884, #18335 ) ;
#7070 = DIRECTION ( 'NONE',  ( 0.8916010070300383061, -0.4528218681369324261, 0.000000000000000000 ) ) ;
#7071 = FACE_OUTER_BOUND ( 'NONE', #22123, .T. ) ;
#7072 = ORIENTED_EDGE ( 'NONE', *, *, #912, .T. ) ;
#7073 = DIRECTION ( 'NONE',  ( 0.000000000000000000, 0.000000000000000000, 1.000000000000000000 ) ) ;
#7074 = ORIENTED_EDGE ( 'NONE', *, *, #26401, .F. ) ;
#7075 = EDGE_CURVE ( 'NONE', #16487, #5204, #17438, .T. ) ;
#7076 = EDGE_CURVE ( 'NONE', #26636, #22380, #12512, .T. ) ;
#7077 =( REPRESENTATION_RELATIONSHIP ('NONE','NONE', #11963, #14145 ) REPRESENTATION_RELATIONSHIP_WITH_TRANSFORMATION ( #9347 )SHAPE_REPRESENTATION_RELATIONSHIP( ) );
#7078 = FACE_OUTER_BOUND ( 'NONE', #8252, .T. ) ;
#7079 = CARTESIAN_POINT ( 'NONE',  ( 216.4313787033304379, 124.9567147554451623, 45.00000000000000000 ) ) ;
#7080 = ORIENTED_EDGE ( 'NONE', *, *, #169, .T. ) ;
#7081 = VECTOR ( 'NONE', #20124, 1000.000000000000000 ) ;
#7082 = VERTEX_POINT ( 'NONE', #10908 ) ;
#7083 = DIRECTION ( 'NONE',  ( 0.000000000000000000, 0.000000000000000000, -1.000000000000000000 ) ) ;
#7084 = DIRECTION ( 'NONE',  ( 0.05364526231776645809, -0.9985600561963501320, 0.000000000000000000 ) ) ;
#7085 = VERTEX_POINT ( 'NONE', #8895 ) ;
#7086 = DIRECTION ( 'NONE',  ( 1.000000000000000000, 0.000000000000000000, -0.000000000000000000 ) ) ;
#7087 = VERTEX_POINT ( 'NONE', #6595 ) ;
#7088 = AXIS2_PLACEMENT_3D ( 'NONE', #27511, #12033, #16344 ) ;
#7089 = DIRECTION ( 'NONE',  ( -0.8916010070293484135, 0.4528218681382909505, 0.000000000000000000 ) ) ;
#7090 = CARTESIAN_POINT ( 'NONE',  ( -260.0000000000001137, -170.0000000000001137, -59.99999999999986500 ) ) ;
#7091 = CARTESIAN_POINT ( 'NONE',  ( 158.0000000000001705, 188.9054999099155054, 45.00000000000000000 ) ) ;
#7092 = CARTESIAN_POINT ( 'NONE',  ( -11.66034562843645439, 131.4488408685630247, -14.75304520776273876 ) ) ;
#7093 = FACE_OUTER_BOUND ( 'NONE', #26477, .T. ) ;
#7094 = EDGE_CURVE ( 'NONE', #26492, #18389, #26406, .T. ) ;
#7095 = LINE ( 'NONE', #20453, #11958 ) ;
#7096 = CARTESIAN_POINT ( 'NONE',  ( -40.40953891503691153, 0.000000000000000000, 99.00000000000000000 ) ) ;
#7097 = VERTEX_POINT ( 'NONE', #4146 ) ;
#7098 = EDGE_CURVE ( 'NONE', #7888, #6230, #129, .T. ) ;
#7099 = LINE ( 'NONE', #13721, #21009 ) ;
#7100 = PLANE ( 'NONE',  #3744 ) ;
#7101 = CARTESIAN_POINT ( 'NONE',  ( 158.0000000000009663, 113.6692496847042264, -45.00000000000000000 ) ) ;
#7102 = LINE ( 'NONE', #11281, #21728 ) ;
#7103 = ORIENTED_EDGE ( 'NONE', *, *, #13325, .F. ) ;
#7104 = VECTOR ( 'NONE', #8898, 1000.000000000000000 ) ;
#7105 = DIRECTION ( 'NONE',  ( -0.8916010070298968637, -0.4528218681372109811, 0.000000000000000000 ) ) ;
#7106 = EDGE_LOOP ( 'NONE', ( #26139, #8434, #16830, #3855, #27548, #19177, #4502, #6048, #3037, #20566, #24793, #21013, #26534, #21517, #22899, #3060 ) ) ;
#7107 = CARTESIAN_POINT ( 'NONE',  ( 157.4999999999996874, 268.9035626463865469, 45.00000000000000000 ) ) ;
#7108 = CARTESIAN_POINT ( 'NONE',  ( -218.0684950290402071, 60.60891383183041370, -12.02124378490089285 ) ) ;
#7109 = CYLINDRICAL_SURFACE ( 'NONE', #16312, 16.07743405327025243 ) ;
#7110 = EDGE_LOOP ( 'NONE', ( #19014, #2314, #10295, #2441 ) ) ;
#7111 = CARTESIAN_POINT ( 'NONE',  ( 136.0000000000000853, 196.9999999999997442, 45.00000000000000000 ) ) ;
#7112 = DIRECTION ( 'NONE',  ( 0.000000000000000000, 0.000000000000000000, 1.000000000000000000 ) ) ;
#7113 = VECTOR ( 'NONE', #24174, 1000.000000000000000 ) ;
#7114 = VERTEX_POINT ( 'NONE', #19241 ) ;
#7115 = CARTESIAN_POINT ( 'NONE',  ( -211.5723746692770817, 73.07838658328543602, 31.37812082757087495 ) ) ;
#7116 = ORIENTED_EDGE ( 'NONE', *, *, #20387, .T. ) ;
#7117 = CARTESIAN_POINT ( 'NONE',  ( 158.0000000000004263, 166.3346248423521274, 45.00000000000000000 ) ) ;
#7118 = ORIENTED_EDGE ( 'NONE', *, *, #1800, .F. ) ;
#7119 = ADVANCED_FACE ( 'NONE', ( #25844 ), #13215, .T. ) ;
#7120 = VERTEX_POINT ( 'NONE', #26269 ) ;
#7121 = EDGE_CURVE ( 'NONE', #14063, #16893, #1848, .T. ) ;
#7122 = FACE_OUTER_BOUND ( 'NONE', #3966, .T. ) ;
#7123 = ORIENTED_EDGE ( 'NONE', *, *, #24060, .F. ) ;
#7124 = VECTOR ( 'NONE', #9285, 1000.000000000000114 ) ;
#7125 = EDGE_CURVE ( 'NONE', #18109, #11335, #21681, .T. ) ;
#7126 = VERTEX_POINT ( 'NONE', #15084 ) ;
#7127 = ORIENTED_EDGE ( 'NONE', *, *, #149, .T. ) ;
#7128 = CARTESIAN_POINT ( 'NONE',  ( 106.0806716804939356, 248.0923932631196749, 24.09863730004343552 ) ) ;
#7129 = CARTESIAN_POINT ( 'NONE',  ( 158.0000000000015916, 55.48024950453520177, -45.00000000000000000 ) ) ;
#7130 = PLANE ( 'NONE',  #16089 ) ;
#7131 = AXIS2_PLACEMENT_3D ( 'NONE', #15442, #25912, #15302 ) ;
#7132 = DIRECTION ( 'NONE',  ( 0.000000000000000000, -1.000000000000000000, 0.000000000000000000 ) ) ;
#7133 = DIRECTION ( 'NONE',  ( 0.000000000000000000, 1.000000000000000000, -0.000000000000000000 ) ) ;
#7134 = CARTESIAN_POINT ( 'NONE',  ( 65.00000000000000000, -120.0250000000000909, -63.99999999999998579 ) ) ;
#7135 = CARTESIAN_POINT ( 'NONE',  ( 158.0000000000006821, 138.7479997597746433, -45.00000000000000000 ) ) ;
#7136 = CARTESIAN_POINT ( 'NONE',  ( 158.0000000000011937, 91.09837461714084839, 45.00000000000000000 ) ) ;
#7137 = CARTESIAN_POINT ( 'NONE',  ( 158.0000000000012221, 90.59049960963380954, 45.00000000000000000 ) ) ;
#7138 = DIRECTION ( 'NONE',  ( -4.625929269271489858E-16, 2.100614451407711032E-31, -1.000000000000000000 ) ) ;
#7139 = CARTESIAN_POINT ( 'NONE',  ( 132.3894761555990556, 200.1711027725235397, 45.00000000000000000 ) ) ;
#7140 = VERTEX_POINT ( 'NONE', #4296 ) ;
#7141 = FACE_OUTER_BOUND ( 'NONE', #15182, .T. ) ;
#7142 = FACE_OUTER_BOUND ( 'NONE', #13631, .T. ) ;
#7143 = DIRECTION ( 'NONE',  ( 0.000000000000000000, 0.000000000000000000, -1.000000000000000000 ) ) ;
#7144 = VECTOR ( 'NONE', #8813, 1000.000000000000227 ) ;
#7145 = CARTESIAN_POINT ( 'NONE',  ( 108.6344068260611948, 205.6858709818343982, -139.0484678162420948 ) ) ;
#7146 = ORIENTED_EDGE ( 'NONE', *, *, #9496, .T. ) ;
#7147 = CIRCLE ( 'NONE', #12672, 11.00000000000001066 ) ;
#7148 = CIRCLE ( 'NONE', #19078, 5.000000000000004441 ) ;
#7149 = DIRECTION ( 'NONE',  ( -1.000000000000000000, 0.000000000000000000, -0.000000000000000000 ) ) ;
#7150 = ORIENTED_EDGE ( 'NONE', *, *, #7918, .T. ) ;
#7151 = DIRECTION ( 'NONE',  ( -0.8916010070297041290, -0.4528218681375906218, 0.000000000000000000 ) ) ;
#7152 = ADVANCED_FACE ( 'NONE', ( #8471 ), #19530, .F. ) ;
#7153 = VECTOR ( 'NONE', #28000, 1000.000000000000000 ) ;
#7154 = VERTEX_POINT ( 'NONE', #10481 ) ;
#7155 = EDGE_CURVE ( 'NONE', #24989, #26858, #27988, .T. ) ;
#7156 = EDGE_CURVE ( 'NONE', #3350, #627, #6168, .T. ) ;
#7157 = ORIENTED_EDGE ( 'NONE', *, *, #25981, .T. ) ;
#7158 = ORIENTED_EDGE ( 'NONE', *, *, #22289, .T. ) ;
#7159 = VERTEX_POINT ( 'NONE', #17503 ) ;
#7160 = CARTESIAN_POINT ( 'NONE',  ( 28.57744295357075259, -14.51376905457599342, 45.00000000000000000 ) ) ;
#7161 = CARTESIAN_POINT ( 'NONE',  ( 65.00000000000000000, -120.0250000000000909, -69.99999999999998579 ) ) ;
#7162 = CARTESIAN_POINT ( 'NONE',  ( 158.0000000000007105, 138.2401247522676044, -45.00000000000000000 ) ) ;
#7163 = PLANE ( 'NONE',  #22936 ) ;
#7164 = VECTOR ( 'NONE', #13793, 1000.000000000000114 ) ;
#7165 = PRODUCT_DEFINITION_CONTEXT ( 'detailed design', #24702, 'design' ) ;
#7166 = VECTOR ( 'NONE', #19904, 1000.000000000000000 ) ;
#7167 = FACE_OUTER_BOUND ( 'NONE', #22155, .T. ) ;
#7168 = CARTESIAN_POINT ( 'NONE',  ( -228.8737713456696952, 63.73618850396876923, 17.32239903714441809 ) ) ;
#7169 = DIRECTION ( 'NONE',  ( 0.7440215159219069063, 0.6681556583950086781, 0.000000000000000000 ) ) ;
#7170 = LINE ( 'NONE', #20234, #11297 ) ;
#7171 = CARTESIAN_POINT ( 'NONE',  ( 79.99999999999997158, 83.92694226569396676, -99.80661736361717828 ) ) ;
#7172 = CARTESIAN_POINT ( 'NONE',  ( -206.8654573299152162, 90.47654849149037659, -26.13928083963914517 ) ) ;
#7173 =( BOUNDED_SURFACE ( )  B_SPLINE_SURFACE ( 3, 2, ( 
 ( #19248, #25849, #23703 ),
 ( #19812, #28399, #6174 ),
 ( #17511, #27992, #26280 ),
 ( #14951, #4438, #21968 ),
 ( #4009, #12796, #1852 ),
 ( #15522, #2280, #8477 ),
 ( #11058, #3872, #17232 ),
 ( #25991, #6310, #15088 ),
 ( #2000, #9484, #23078 ),
 ( #1236, #20386, #10003 ),
 ( #5009, #18098, #572 ),
 ( #3384, #26853, #7322 ),
 ( #12173, #15949, #20916 ),
 ( #19958, #9336, #16475 ),
 ( #9192, #18760, #11649 ),
 ( #13801, #6884, #25226 ),
 ( #14320, #5545, #27509 ),
 ( #7842, #13364, #15663 ),
 ( #24269, #20097, #4578 ),
 ( #22256, #24557, #7032 ),
 ( #22547, #26989, #22113 ),
 ( #24703, #2421, #9045 ),
 ( #26554, #17798, #4722 ),
 ( #24411, #2858, #429 ) ),
 .UNSPECIFIED., .F., .F., .T. ) 
 B_SPLINE_SURFACE_WITH_KNOTS ( ( 4, 2, 2, 2, 2, 2, 2, 2, 2, 2, 2, 4 ),
 ( 3, 3 ),
 ( 0.000000000000000000, 0.006931781491214596483, 0.01386356298242919297, 0.01732945372803649381, 0.02079534447364379118, 0.02772712596485838593, 0.03465890745607298762, 0.03639185282887663631, 0.03812479820168028499, 0.04159068894728758237, 0.04852247043850217711, 0.05545425192971677186 ),
 ( 0.000000000000000000, 1.000000000000000000 ),
 .UNSPECIFIED. ) 
 GEOMETRIC_REPRESENTATION_ITEM ( )  RATIONAL_B_SPLINE_SURFACE ( (
 ( 1.000000000000000000, 0.8161343730438194166, 1.000000000000000000),
 ( 1.000000000000000000, 0.8224195403628062895, 1.000000000000000000),
 ( 1.000000000000000000, 0.8273233292672230732, 1.000000000000000000),
 ( 1.000000000000000000, 0.8342607332264897479, 1.000000000000000000),
 ( 1.000000000000000000, 0.8362950954338710385, 1.000000000000000000),
 ( 1.000000000000000000, 0.8371032263789185413, 1.000000000000000000),
 ( 1.000000000000000000, 0.8369960692425010285, 1.000000000000000000),
 ( 1.000000000000000000, 0.8360286494151781822, 1.000000000000000000),
 ( 1.000000000000000000, 0.8351716839152490968, 1.000000000000000000),
 ( 1.000000000000000000, 0.8315174131673371827, 1.000000000000000000),
 ( 1.000000000000000000, 0.8276373651588401215, 1.000000000000000000),
 ( 1.000000000000000000, 0.8171610397916245772, 1.000000000000000000),
 ( 1.000000000000000000, 0.8105635768882419878, 1.000000000000000000),
 ( 1.000000000000000000, 0.8007212358742062941, 1.000000000000000000),
 ( 1.000000000000000000, 0.7986706403516325992, 1.000000000000000000),
 ( 1.000000000000000000, 0.7944384422229460174, 1.000000000000000000),
 ( 1.000000000000000000, 0.7922545277786539053, 1.000000000000000000),
 ( 1.000000000000000000, 0.7855097680936570237, 1.000000000000000000),
 ( 1.000000000000000000, 0.7807558079320371380, 1.000000000000000000),
 ( 1.000000000000000000, 0.7658071389224905268, 1.000000000000000000),
 ( 1.000000000000000000, 0.7549214566164625939, 1.000000000000000000),
 ( 1.000000000000000000, 0.7318315617936779205, 1.000000000000000000),
 ( 1.000000000000000000, 0.7196266900043837289, 1.000000000000000000),
 ( 1.000000000000000000, 0.7071067811865477948, 1.000000000000000000) ) ) 
 REPRESENTATION_ITEM ( '' )  SURFACE ( )  );
#7174 = AXIS2_PLACEMENT_3D ( 'NONE', #25813, #6141, #13465 ) ;
#7175 = CARTESIAN_POINT ( 'NONE',  ( 158.0000000000000568, 201.4448749474510407, -45.00000000000000000 ) ) ;
#7176 = DIRECTION ( 'NONE',  ( -0.8916010070296834789, 0.4528218681376311450, 0.000000000000000000 ) ) ;
#7177 = CARTESIAN_POINT ( 'NONE',  ( -200.0000000000000284, -120.0000000000001279, 25.00000000000000000 ) ) ;
#7178 = CARTESIAN_POINT ( 'NONE',  ( 157.9999999999996874, 271.1575001501400379, 45.00000000000000000 ) ) ;
#7179 = LINE ( 'NONE', #7608, #27482 ) ;
#7180 = CARTESIAN_POINT ( 'NONE',  ( -161.9363290404624820, 118.9535531856865163, 23.59303681828691879 ) ) ;
#7181 = DIRECTION ( 'NONE',  ( 0.000000000000000000, -1.000000000000000000, 0.000000000000000000 ) ) ;
#7183 = ORIENTED_EDGE ( 'NONE', *, *, #24018, .F. ) ;
#7182 = ORIENTED_EDGE ( 'NONE', *, *, #14822, .T. ) ;
#7184 = CARTESIAN_POINT ( 'NONE',  ( 158.0000000000015064, 61.00387452705632541, 45.00000000000000000 ) ) ;
#7185 = EDGE_CURVE ( 'NONE', #27375, #25233, #23699, .T. ) ;
#7186 = CARTESIAN_POINT ( 'NONE',  ( 157.4999999999998579, 68.27356204582390831, -45.00000000000000000 ) ) ;
#7187 = ORIENTED_EDGE ( 'NONE', *, *, #7657, .F. ) ;
#7188 = CONTEXT_DEPENDENT_SHAPE_REPRESENTATION ( #11501, #15098 ) ;
#7189 = ORIENTED_EDGE ( 'NONE', *, *, #15983, .T. ) ;
#7190 = VECTOR ( 'NONE', #19587, 1000.000000000000114 ) ;
#7191 = ORIENTED_EDGE ( 'NONE', *, *, #14545, .T. ) ;
#7192 = EDGE_CURVE ( 'NONE', #3012, #968, #1994, .T. ) ;
#7193 = DIRECTION ( 'NONE',  ( 0.000000000000000000, 0.000000000000000000, -1.000000000000000000 ) ) ;
#7194 = CARTESIAN_POINT ( 'NONE',  ( -133.8788553768147267, 130.0499255244862127, 16.66544065180372414 ) ) ;
#7195 = EDGE_CURVE ( 'NONE', #3903, #20000, #26125, .T. ) ;
#7196 = ORIENTED_EDGE ( 'NONE', *, *, #17292, .F. ) ;
#7197 = VECTOR ( 'NONE', #2960, 1000.000000000000000 ) ;
#7198 = EDGE_LOOP ( 'NONE', ( #1593, #1837, #13854, #6684 ) ) ;
#7199 = CARTESIAN_POINT ( 'NONE',  ( 157.9999999999998579, 0.000000000000000000, 45.00000000000000000 ) ) ;
#7200 = CARTESIAN_POINT ( 'NONE',  ( 179.9999999999999147, 330.0000000000000000, 100.0000000000000142 ) ) ;
#7201 = CARTESIAN_POINT ( 'NONE',  ( 157.9999999999996305, 284.2047501951820436, 45.00000000000000000 ) ) ;
#7202 = ORIENTED_EDGE ( 'NONE', *, *, #10850, .F. ) ;
#7203 = DIRECTION ( 'NONE',  ( 0.000000000000000000, 1.000000000000000000, -0.000000000000000000 ) ) ;
#7204 = LINE ( 'NONE', #11528, #8421 ) ;
#7205 = DIRECTION ( 'NONE',  ( -1.000000000000000000, 0.000000000000000000, 0.000000000000000000 ) ) ;
#7206 = FACE_OUTER_BOUND ( 'NONE', #17282, .T. ) ;
#7207 = AXIS2_PLACEMENT_3D ( 'NONE', #7894, #18537, #1144 ) ;
#7208 = CARTESIAN_POINT ( 'NONE',  ( -213.4585383333369180, 57.78353604556345857, -35.98283585097398429 ) ) ;
#7209 = CIRCLE ( 'NONE', #23264, 43.76444293738737912 ) ;
#7210 = DIRECTION ( 'NONE',  ( 0.000000000000000000, 0.000000000000000000, -1.000000000000000000 ) ) ;
#7211 = EDGE_CURVE ( 'NONE', #17167, #21241, #17225, .T. ) ;
#7212 = CARTESIAN_POINT ( 'NONE',  ( -227.3657730843038678, 133.9833936510422632, -14.99191580167116378 ) ) ;
#7213 = LINE ( 'NONE', #27162, #11124 ) ;
#7214 = CARTESIAN_POINT ( 'NONE',  ( 158.0000000000014779, 65.51174953456337846, -45.00000000000000000 ) ) ;
#7215 = EDGE_LOOP ( 'NONE', ( #11969, #18305, #8692, #10506 ) ) ;
#7216 = DIRECTION ( 'NONE',  ( -0.000000000000000000, -0.000000000000000000, -1.000000000000000000 ) ) ;
#7217 = EDGE_CURVE ( 'NONE', #543, #12064, #11052, .T. ) ;
#7218 = CARTESIAN_POINT ( 'NONE',  ( -40.40953891503691153, 71.03850157808263077, 99.00000000000000000 ) ) ;
#7219 = CARTESIAN_POINT ( 'NONE',  ( 157.4999999999995737, 203.6988124512014338, -45.00000000000000000 ) ) ;
#7220 = ORIENTED_EDGE ( 'NONE', *, *, #22633, .T. ) ;
#7221 = DIRECTION ( 'NONE',  ( 0.000000000000000000, 0.000000000000000000, 1.000000000000000000 ) ) ;
#7222 = EDGE_LOOP ( 'NONE', ( #10644, #17277, #26749, #2333 ) ) ;
#7223 = DIRECTION ( 'NONE',  ( 1.000000000000000000, -0.000000000000000000, -0.000000000000000000 ) ) ;
#7224 = CARTESIAN_POINT ( 'NONE',  ( 232.4999999999996305, 133.0668745871126930, -42.88984227207694744 ) ) ;
#7225 = EDGE_CURVE ( 'NONE', #12854, #12943, #21828, .T. ) ;
#7226 = VERTEX_POINT ( 'NONE', #22369 ) ;
#7227 = CIRCLE ( 'NONE', #19585, 2.000000000000007550 ) ;
#7228 = VERTEX_POINT ( 'NONE', #17481 ) ;
#7229 = CARTESIAN_POINT ( 'NONE',  ( 179.9999999999999147, 494.4107529906318632, 100.0000000000000142 ) ) ;
#7230 = AXIS2_PLACEMENT_3D ( 'NONE', #13783, #3256, #12049 ) ;
#7231 = EDGE_CURVE ( 'NONE', #4081, #10866, #17913, .T. ) ;
#7232 = PLANE ( 'NONE',  #17532 ) ;
#7233 = ORIENTED_EDGE ( 'NONE', *, *, #3339, .T. ) ;
#7234 = FACE_OUTER_BOUND ( 'NONE', #22765, .T. ) ;
#7235 = ORIENTED_EDGE ( 'NONE', *, *, #13540, .T. ) ;
#7236 = DIRECTION ( 'NONE',  ( -0.000000000000000000, -1.000000000000000000, -0.000000000000000000 ) ) ;
#7237 = DIRECTION ( 'NONE',  ( 1.000000000000000000, -0.000000000000000000, -0.000000000000000000 ) ) ;
#7238 = DIRECTION ( 'NONE',  ( 1.000000000000000000, -0.000000000000000000, -0.000000000000000000 ) ) ;
#7239 = CARTESIAN_POINT ( 'NONE',  ( -13.66674585099290873, 130.9048851640479825, -16.37515642400365579 ) ) ;
#7240 = PLANE ( 'NONE',  #16457 ) ;
#7241 = EDGE_CURVE ( 'NONE', #23120, #5724, #4408, .T. ) ;
#7242 = DIRECTION ( 'NONE',  ( 0.4528218681382319422, 0.8916010070293783896, -0.000000000000000000 ) ) ;
#7243 = DIRECTION ( 'NONE',  ( -0.000000000000000000, 0.000000000000000000, -1.000000000000000000 ) ) ;
#7244 = ORIENTED_EDGE ( 'NONE', *, *, #11680, .T. ) ;
#7245 = DIRECTION ( 'NONE',  ( 0.000000000000000000, 0.000000000000000000, 1.000000000000000000 ) ) ;
#7246 = CARTESIAN_POINT ( 'NONE',  ( 157.4999999999998295, 228.7775625262745223, 45.00000000000000000 ) ) ;
#7247 = PLANE ( 'NONE',  #22882 ) ;
#7248 = DIRECTION ( 'NONE',  ( 0.000000000000000000, 0.000000000000000000, 1.000000000000000000 ) ) ;
#7249 = ORIENTED_EDGE ( 'NONE', *, *, #16464, .F. ) ;
#7250 = DIRECTION ( 'NONE',  ( 1.000000000000000000, -0.000000000000000000, -0.000000000000000000 ) ) ;
#7251 = AXIS2_PLACEMENT_3D ( 'NONE', #13853, #13040, #10733 ) ;
#7252 = ORIENTED_EDGE ( 'NONE', *, *, #13358, .F. ) ;
#7253 = ADVANCED_FACE ( 'NONE', ( #6428 ), #26663, .F. ) ;
#7254 = CARTESIAN_POINT ( 'NONE',  ( 135.9999999999998295, 242.9999999999997158, 45.00000000000000000 ) ) ;
#7255 = CYLINDRICAL_SURFACE ( 'NONE', #12846, 24.07986109634097005 ) ;
#7256 = DIRECTION ( 'NONE',  ( 0.000000000000000000, -0.000000000000000000, -1.000000000000000000 ) ) ;
#7257 = VERTEX_POINT ( 'NONE', #24105 ) ;
#7258 = DIRECTION ( 'NONE',  ( -0.000000000000000000, -0.000000000000000000, 1.000000000000000000 ) ) ;
#7259 = CARTESIAN_POINT ( 'NONE',  ( 157.4999999999994600, 213.7303124812313513, 45.00000000000000000 ) ) ;
#7260 = EDGE_LOOP ( 'NONE', ( #23470, #26147, #17464, #266, #21262, #16489 ) ) ;
#7261 = CARTESIAN_POINT ( 'NONE',  ( 157.9999999999997442, 251.0945000900840398, 45.00000000000000000 ) ) ;
#7262 = ORIENTED_EDGE ( 'NONE', *, *, #9265, .F. ) ;
#7263 = CARTESIAN_POINT ( 'NONE',  ( -233.2943309833541718, 92.06151970357193193, -15.00000000000000000 ) ) ;
#7264 = ORIENTED_EDGE ( 'NONE', *, *, #18057, .F. ) ;
#7265 = ORIENTED_EDGE ( 'NONE', *, *, #10390, .F. ) ;
#7266 = EDGE_CURVE ( 'NONE', #24350, #28186, #4831, .T. ) ;
#7267 = DIRECTION ( 'NONE',  ( -0.000000000000000000, 0.000000000000000000, -1.000000000000000000 ) ) ;
#7268 = ORIENTED_EDGE ( 'NONE', *, *, #11735, .T. ) ;
#7269 = ADVANCED_FACE ( 'NONE', ( #6848 ), #26516, .F. ) ;
#7270 = AXIS2_PLACEMENT_3D ( 'NONE', #18167, #26920, #12413 ) ;
#7271 = ORIENTED_EDGE ( 'NONE', *, *, #4602, .F. ) ;
#7272 = EDGE_LOOP ( 'NONE', ( #15212, #22647 ) ) ;
#7273 = FACE_OUTER_BOUND ( 'NONE', #7858, .T. ) ;
#7274 = CARTESIAN_POINT ( 'NONE',  ( 158.0000000000005400, 158.3031248123239436, 45.00000000000000000 ) ) ;
#7275 = LINE ( 'NONE', #20199, #5952 ) ;
#7276 = ADVANCED_FACE ( 'NONE', ( #15205 ), #15490, .F. ) ;
#7277 = CARTESIAN_POINT ( 'NONE',  ( 232.4999999999996305, 44.41075299063185611, -75.35061095560293154 ) ) ;
#7278 = CARTESIAN_POINT ( 'NONE',  ( -175.0000000000000000, -170.0000000000001705, 70.00000000000001421 ) ) ;
#7279 = DIRECTION ( 'NONE',  ( 1.000000000000000000, 0.000000000000000000, 0.000000000000000000 ) ) ;
#7280 =( GEOMETRIC_REPRESENTATION_CONTEXT ( 3 ) GLOBAL_UNCERTAINTY_ASSIGNED_CONTEXT ( ( #11776 ) ) GLOBAL_UNIT_ASSIGNED_CONTEXT ( ( #25645, #23643, #10571 ) ) REPRESENTATION_CONTEXT ( 'NONE', 'WORKASPACE' ) );
#7281 = FACE_OUTER_BOUND ( 'NONE', #11028, .T. ) ;
#7282 = DIRECTION ( 'NONE',  ( 0.4528218681369324261, 0.8916010070300384172, -0.000000000000000000 ) ) ;
#7283 = LINE ( 'NONE', #20632, #4179 ) ;
#7284 = CYLINDRICAL_SURFACE ( 'NONE', #13711, 2.000000000000003109 ) ;
#7285 = DIRECTION ( 'NONE',  ( -0.000000000000000000, -0.000000000000000000, -1.000000000000000000 ) ) ;
#7286 = ORIENTED_EDGE ( 'NONE', *, *, #2343, .T. ) ;
#7287 = CARTESIAN_POINT ( 'NONE',  ( 0.000000000000000000, 242.9999999999997158, -45.00000000000000000 ) ) ;
#7288 = EDGE_CURVE ( 'NONE', #22168, #26591, #492, .T. ) ;
#7289 = CIRCLE ( 'NONE', #10477, 80.00000000000000000 ) ;
#7290 = AXIS2_PLACEMENT_3D ( 'NONE', #16778, #7870, #22824 ) ;
#7291 = CARTESIAN_POINT ( 'NONE',  ( 158.0000000000014495, 66.01962454207041731, 45.00000000000000000 ) ) ;
#7292 = LINE ( 'NONE', #24670, #28166 ) ;
#7293 = ADVANCED_FACE ( 'NONE', ( #4544 ), #6002, .T. ) ;
#7294 = CARTESIAN_POINT ( 'NONE',  ( 65.00000000000000000, -120.0000000000000711, 64.00000000000002842 ) ) ;
#7295 = ORIENTED_EDGE ( 'NONE', *, *, #8807, .T. ) ;
#7296 = DIRECTION ( 'NONE',  ( 0.8916010070293783896, -0.4528218681382319422, 0.000000000000000000 ) ) ;
#7297 = VERTEX_POINT ( 'NONE', #28249 ) ;
#7298 = LINE ( 'NONE', #3107, #17806 ) ;
#7299 = ORIENTED_EDGE ( 'NONE', *, *, #24814, .F. ) ;
#7300 = VECTOR ( 'NONE', #16675, 1000.000000000000000 ) ;
#7301 = EDGE_LOOP ( 'NONE', ( #14233, #13066, #8994, #1209 ) ) ;
#7302 = ORIENTED_EDGE ( 'NONE', *, *, #15183, .T. ) ;
#7303 = VERTEX_POINT ( 'NONE', #11029 ) ;
#7304 = DIRECTION ( 'NONE',  ( 0.000000000000000000, 0.000000000000000000, 1.000000000000000000 ) ) ;
#7305 = CARTESIAN_POINT ( 'NONE',  ( 157.4999999999995453, 206.2066874587088989, -45.00000000000000000 ) ) ;
#7306 = CARTESIAN_POINT ( 'NONE',  ( 217.4999999999996305, 258.6181251126050711, -6.024999999999988809 ) ) ;
#7307 = AXIS2_PLACEMENT_3D ( 'NONE', #26781, #2781, #4500 ) ;
#7308 = CARTESIAN_POINT ( 'NONE',  ( -52.83157022077657672, 131.8429468099762687, -16.11955406963874537 ) ) ;
#7309 = CARTESIAN_POINT ( 'NONE',  ( 158.0000000000010800, 103.1298746471690038, 45.00000000000000000 ) ) ;
#7310 = AXIS2_PLACEMENT_3D ( 'NONE', #14128, #7373, #24897 ) ;
#7311 = CARTESIAN_POINT ( 'NONE',  ( -213.2358879321101313, 57.03087831670950436, 38.93822867433466683 ) ) ;
#7312 = DIRECTION ( 'NONE',  ( -0.000000000000000000, -0.000000000000000000, -1.000000000000000000 ) ) ;
#7313 = DIRECTION ( 'NONE',  ( 1.000000000000000000, 0.000000000000000000, 0.000000000000000000 ) ) ;
#7314 = CARTESIAN_POINT ( 'NONE',  ( 157.4999999999997726, 246.3326875788235384, 45.00000000000000000 ) ) ;
#7315 = FACE_OUTER_BOUND ( 'NONE', #10046, .T. ) ;
#7316 = EDGE_CURVE ( 'NONE', #6014, #27664, #26379, .T. ) ;
#7317 = DIRECTION ( 'NONE',  ( 1.000000000000000000, 0.000000000000000000, 0.000000000000000000 ) ) ;
#7318 = CARTESIAN_POINT ( 'NONE',  ( -79.00187704905530950, 96.44595867864546790, -145.0000000000000000 ) ) ;
#7319 = CARTESIAN_POINT ( 'NONE',  ( 84.91648909967247505, 110.3843228249417479, 70.37109374985131183 ) ) ;
#7320 = ADVANCED_FACE ( 'NONE', ( #2247 ), #26245, .T. ) ;
#7322 = CARTESIAN_POINT ( 'NONE',  ( -13.76547155678103707, 130.8815623877831911, 14.96787615611629541 ) ) ;
#7321 = VECTOR ( 'NONE', #28031, 1000.000000000000227 ) ;
#7323 = DIRECTION ( 'NONE',  ( 0.000000000000000000, 0.000000000000000000, -1.000000000000000000 ) ) ;
#7324 =( GEOMETRIC_REPRESENTATION_CONTEXT ( 3 ) GLOBAL_UNCERTAINTY_ASSIGNED_CONTEXT ( ( #4852 ) ) GLOBAL_UNIT_ASSIGNED_CONTEXT ( ( #24383, #17774, #6581 ) ) REPRESENTATION_CONTEXT ( 'NONE', 'WORKASPACE' ) );
#7325 = CARTESIAN_POINT ( 'NONE',  ( -191.5097071395943544, 102.0944051927142340, 32.85252593193306581 ) ) ;
#7326 = DIRECTION ( 'NONE',  ( 0.000000000000000000, 0.000000000000000000, -1.000000000000000000 ) ) ;
#7328 = VERTEX_POINT ( 'NONE', #22081 ) ;
#7327 = ORIENTED_EDGE ( 'NONE', *, *, #12776, .F. ) ;
#7329 = CARTESIAN_POINT ( 'NONE',  ( 157.4999999999998579, 45.70268697826052318, 45.00000000000000000 ) ) ;
#7330 = CIRCLE ( 'NONE', #2258, 45.00000000000000711 ) ;
#7331 = CARTESIAN_POINT ( 'NONE',  ( 33.10302365956999182, 203.2034914284457159, -13.00000000000000000 ) ) ;
#7332 = VERTEX_POINT ( 'NONE', #6993 ) ;
#7333 = ITEM_DEFINED_TRANSFORMATION ( 'NONE', 'NONE', #3751,  #10637 ) ;
#7335 = ORIENTED_EDGE ( 'NONE', *, *, #4873, .T. ) ;
#7334 = AXIS2_PLACEMENT_3D ( 'NONE', #16256, #10058, #5180 ) ;
#7336 = FACE_OUTER_BOUND ( 'NONE', #4599, .T. ) ;
#7337 = CARTESIAN_POINT ( 'NONE',  ( 104.9999999999998579, 220.0000000000000284, -169.9999999999999716 ) ) ;
#7338 = ADVANCED_FACE ( 'NONE', ( #26099 ), #105, .F. ) ;
#7339 = ORIENTED_EDGE ( 'NONE', *, *, #15780, .T. ) ;
#7340 = ORIENTED_EDGE ( 'NONE', *, *, #18925, .T. ) ;
#7341 = DIRECTION ( 'NONE',  ( 0.4528218681374511223, -0.8916010070297750723, 0.000000000000000000 ) ) ;
#7342 = DIRECTION ( 'NONE',  ( -0.8916010070294396739, 0.4528218681381114274, 0.000000000000000000 ) ) ;
#7343 = AXIS2_PLACEMENT_3D ( 'NONE', #22586, #15989, #7502 ) ;
#7344 = EDGE_CURVE ( 'NONE', #5313, #22382, #17340, .T. ) ;
#7345 = LINE ( 'NONE', #24864, #9157 ) ;
#7346 = LINE ( 'NONE', #11375, #16490 ) ;
#7347 =( BOUNDED_SURFACE ( )  B_SPLINE_SURFACE ( 3, 2, ( 
 ( #8628, #25567, #8342 ),
 ( #28286, #17101, #17381 ),
 ( #28145, #17240, #3591 ),
 ( #4161, #25998, #4017 ),
 ( #5894, #6039, #12947 ),
 ( #21550, #10499, #21266 ),
 ( #26143, #12386, #15100 ),
 ( #23857, #14667, #21122 ) ),
 .UNSPECIFIED., .F., .F., .F. ) 
 B_SPLINE_SURFACE_WITH_KNOTS ( ( 4, 2, 2, 4 ),
 ( 3, 3 ),
 ( 1.734723475976807094E-18, 0.008853360896355882970, 0.01328004134453382445, 0.01770672179271176594 ),
 ( 0.000000000000000000, 1.000000000000000000 ),
 .UNSPECIFIED. ) 
 GEOMETRIC_REPRESENTATION_ITEM ( )  RATIONAL_B_SPLINE_SURFACE ( (
 ( 1.000000000000000000, 0.7071067811865475727, 1.000000000000000000),
 ( 1.000000000000000000, 0.7125463296805260027, 1.000000000000000000),
 ( 1.000000000000000000, 0.7151690839163242774, 1.000000000000000000),
 ( 1.000000000000000000, 0.7150975281021120233, 1.000000000000000000),
 ( 1.000000000000000000, 0.7144031600608887755, 1.000000000000000000),
 ( 1.000000000000000000, 0.7116947786415229737, 1.000000000000000000),
 ( 1.000000000000000000, 0.7096971281777894047, 1.000000000000000000),
 ( 1.000000000000000000, 0.7071067811865465735, 1.000000000000000000) ) ) 
 REPRESENTATION_ITEM ( '' )  SURFACE ( )  );
#7348 = CARTESIAN_POINT ( 'NONE',  ( 91.02002523439647064, 230.3620959593083342, -17.09244139626534320 ) ) ;
#7349 = VECTOR ( 'NONE', #6114, 1000.000000000000000 ) ;
#7350 = DIRECTION ( 'NONE',  ( -0.000000000000000000, -0.000000000000000000, -1.000000000000000000 ) ) ;
#7351 = ADVANCED_FACE ( 'NONE', ( #2387 ), #9012, .F. ) ;
#7352 = DIRECTION ( 'NONE',  ( 0.000000000000000000, 0.000000000000000000, -1.000000000000000000 ) ) ;
#7353 = CARTESIAN_POINT ( 'NONE',  ( -194.6040764069587112, 63.06822542404761123, -40.63350569893458442 ) ) ;
#7354 = ADVANCED_FACE ( 'NONE', ( #10888 ), #19643, .F. ) ;
#7355 = CARTESIAN_POINT ( 'NONE',  ( -279.3160071107327553, -91.18033988749901653, -14.13483123440684253 ) ) ;
#7356 = EDGE_CURVE ( 'NONE', #17304, #23194, #7945, .T. ) ;
#7357 = LINE ( 'NONE', #174, #16569 ) ;
#7358 = DIRECTION ( 'NONE',  ( 1.321694076934710155E-16, -1.000000000000000000, 0.000000000000000000 ) ) ;
#7359 = PLANE ( 'NONE',  #28148 ) ;
#7360 = ORIENTED_EDGE ( 'NONE', *, *, #12545, .T. ) ;
#7361 = DIRECTION ( 'NONE',  ( 0.000000000000000000, 0.000000000000000000, 1.000000000000000000 ) ) ;
#7362 = VECTOR ( 'NONE', #17053, 1000.000000000000000 ) ;
#7363 = CARTESIAN_POINT ( 'NONE',  ( 104.9999999999998579, 220.0000000000000284, -169.9999999999999716 ) ) ;
#7364 = ORIENTED_EDGE ( 'NONE', *, *, #27187, .F. ) ;
#7365 = ORIENTED_EDGE ( 'NONE', *, *, #15435, .F. ) ;
#7366 = AXIS2_PLACEMENT_3D ( 'NONE', #20833, #27704, #3864 ) ;
#7367 = CARTESIAN_POINT ( 'NONE',  ( 105.2480867101079980, 123.6573351780392613, 85.93750000029402258 ) ) ;
#7368 = CARTESIAN_POINT ( 'NONE',  ( -203.2481855153402250, 92.57460631283319685, -29.78692811926998729 ) ) ;
#7369 = ORIENTED_EDGE ( 'NONE', *, *, #22916, .T. ) ;
#7370 = VERTEX_POINT ( 'NONE', #5649 ) ;
#7371 = FACE_OUTER_BOUND ( 'NONE', #24890, .T. ) ;
#7372 = CARTESIAN_POINT ( 'NONE',  ( 217.4999999999996305, 194.4107529906318064, 288.0938197134494203 ) ) ;
#7373 = DIRECTION ( 'NONE',  ( 1.000000000000000000, -0.000000000000000000, -0.000000000000000000 ) ) ;
#7374 = ORIENTED_EDGE ( 'NONE', *, *, #19154, .T. ) ;
#7375 = DIRECTION ( 'NONE',  ( -0.000000000000000000, 0.000000000000000000, -1.000000000000000000 ) ) ;
#7376 = ORIENTED_EDGE ( 'NONE', *, *, #9594, .F. ) ;
#7377 = CARTESIAN_POINT ( 'NONE',  ( -210.0000000000000568, -220.0000000000000853, 110.0000000000000284 ) ) ;
#7378 = EDGE_CURVE ( 'NONE', #11333, #28119, #26173, .T. ) ;
#7379 = ADVANCED_FACE ( 'NONE', ( #7141 ), #26821, .T. ) ;
#7380 = AXIS2_PLACEMENT_3D ( 'NONE', #20907, #16193, #14042 ) ;
#7381 = ADVANCED_FACE ( 'NONE', ( #19003 ), #23033, .F. ) ;
#7382 = CARTESIAN_POINT ( 'NONE',  ( 139.9999999999999432, -90.00000000000000000, -100.0000000000000142 ) ) ;
#7383 = DIRECTION ( 'NONE',  ( -0.8916010070299070778, -0.4528218681371909971, 0.000000000000000000 ) ) ;
#7384 = CARTESIAN_POINT ( 'NONE',  ( -28.21136509376883694, 127.9579735385673018, -17.52291426357238535 ) ) ;
#7385 = DIRECTION ( 'NONE',  ( 0.000000000000000000, 0.000000000000000000, 1.000000000000000000 ) ) ;
#7386 = DIRECTION ( 'NONE',  ( -0.8916010070293783896, -0.4528218681382319422, 0.000000000000000000 ) ) ;
#7387 = AXIS2_PLACEMENT_3D ( 'NONE', #17129, #13121, #10811 ) ;
#7388 = LINE ( 'NONE', #24624, #12693 ) ;
#7389 = ORIENTED_EDGE ( 'NONE', *, *, #20600, .T. ) ;
#7390 = DIRECTION ( 'NONE',  ( -0.000000000000000000, -0.000000000000000000, -1.000000000000000000 ) ) ;
#7391 = EDGE_CURVE ( 'NONE', #4479, #2548, #16851, .T. ) ;
#7392 = LINE ( 'NONE', #7670, #23488 ) ;
#7393 = CARTESIAN_POINT ( 'NONE',  ( -277.2150368962633706, -170.0000000000001137, 90.47363622314043141 ) ) ;
#7394 = CARTESIAN_POINT ( 'NONE',  ( 119.9999999999998863, 330.0000000000000000, 100.0000000000000142 ) ) ;
#7395 = VERTEX_POINT ( 'NONE', #26959 ) ;
#7396 = CARTESIAN_POINT ( 'NONE',  ( 157.9999999999997726, 241.5708750675630370, -45.00000000000000000 ) ) ;
#7397 = EDGE_LOOP ( 'NONE', ( #11594, #16984, #12319, #19270 ) ) ;
#7398 = DIRECTION ( 'NONE',  ( 0.9506505318133482429, -0.3102637045530752258, 0.000000000000000000 ) ) ;
#7399 = CARTESIAN_POINT ( 'NONE',  ( -229.6839157287631394, 64.28192771017235430, -7.255073467994252567 ) ) ;
#7401 = VECTOR ( 'NONE', #11942, 1000.000000000000000 ) ;
#7400 = CARTESIAN_POINT ( 'NONE',  ( 158.0000000000013358, 78.55899957960562574, 45.00000000000000000 ) ) ;
#7402 = EDGE_LOOP ( 'NONE', ( #16309, #22052, #7967, #596 ) ) ;
#7403 = LINE ( 'NONE', #7111, #12475 ) ;
#7404 = ORIENTED_EDGE ( 'NONE', *, *, #27605, .T. ) ;
#7405 = CIRCLE ( 'NONE', #24832, 6.025000000000002132 ) ;
#7406 = DIRECTION ( 'NONE',  ( 0.000000000000000000, -1.000000000000000000, 0.000000000000000000 ) ) ;
#7407 = FACE_OUTER_BOUND ( 'NONE', #6721, .T. ) ;
#7408 = ORIENTED_EDGE ( 'NONE', *, *, #6093, .T. ) ;
#7409 = ORIENTED_EDGE ( 'NONE', *, *, #5486, .T. ) ;
#7410 = DIRECTION ( 'NONE',  ( 0.000000000000000000, 0.000000000000000000, -1.000000000000000000 ) ) ;
#7411 = ORIENTED_EDGE ( 'NONE', *, *, #28294, .F. ) ;
#7412 = AXIS2_PLACEMENT_3D ( 'NONE', #6917, #22436, #18131 ) ;
#7413 = ORIENTED_EDGE ( 'NONE', *, *, #28331, .T. ) ;
#7414 = ORIENTED_EDGE ( 'NONE', *, *, #20317, .F. ) ;
#7415 = CARTESIAN_POINT ( 'NONE',  ( 109.9639884628863058, 258.5863491988774854, 43.28603914701826483 ) ) ;
#7416 = EDGE_CURVE ( 'NONE', #24468, #8776, #16549, .T. ) ;
#7417 = CARTESIAN_POINT ( 'NONE',  ( 158.0000000000000284, 203.9527499549551806, 45.00000000000000000 ) ) ;
#7418 = DIRECTION ( 'NONE',  ( -0.000000000000000000, -0.000000000000000000, -1.000000000000000000 ) ) ;
#7419 = LINE ( 'NONE', #27226, #16107 ) ;
#7420 = DIRECTION ( 'NONE',  ( -0.000000000000000000, -0.000000000000000000, 1.000000000000000000 ) ) ;
#7421 = DIRECTION ( 'NONE',  ( 1.000000000000000000, 0.000000000000000000, 0.000000000000000000 ) ) ;
#7422 = VECTOR ( 'NONE', #18205, 1000.000000000000000 ) ;
#7423 = CARTESIAN_POINT ( 'NONE',  ( 158.0000000000009663, 115.6692496847042264, -45.00000000000000000 ) ) ;
#7424 = FACE_OUTER_BOUND ( 'NONE', #17376, .T. ) ;
#7425 = DIRECTION ( 'NONE',  ( -0.000000000000000000, 1.000000000000000000, -1.387778780781445429E-16 ) ) ;
#7426 = CARTESIAN_POINT ( 'NONE',  ( 109.9999999999998863, 330.0000000000000000, -90.00000000000004263 ) ) ;
#7427 = FACE_OUTER_BOUND ( 'NONE', #234, .T. ) ;
#7428=STYLED_ITEM('',(#28455),#28156);
#7429 = EDGE_LOOP ( 'NONE', ( #8226, #18882, #23369, #15894 ) ) ;
#7430 = AXIS2_PLACEMENT_3D ( 'NONE', #27513, #688, #9730 ) ;
#7431 = EDGE_CURVE ( 'NONE', #23450, #9316, #10108, .T. ) ;
#7432 = EDGE_CURVE ( 'NONE', #7126, #10815, #20877, .T. ) ;
#7433 = CARTESIAN_POINT ( 'NONE',  ( -237.3870311360068683, 121.7710280244218524, -13.00000000000000000 ) ) ;
#7434 = CARTESIAN_POINT ( 'NONE',  ( -189.5231184314577604, 157.6231267382823376, 12.99999999999999822 ) ) ;
#7435 = CARTESIAN_POINT ( 'NONE',  ( 232.4999999999996305, 194.4107529906318064, 75.35061095560297417 ) ) ;
#7436 = ORIENTED_EDGE ( 'NONE', *, *, #28125, .F. ) ;
#7437 = CARTESIAN_POINT ( 'NONE',  ( 157.4999999999998579, 88.33656210588026170, 45.00000000000000000 ) ) ;
#7438 = ORIENTED_EDGE ( 'NONE', *, *, #5988, .F. ) ;
#7439 = DIRECTION ( 'NONE',  ( 1.000000000000000000, -0.000000000000000000, 0.000000000000000000 ) ) ;
#7440 = EDGE_CURVE ( 'NONE', #2977, #7154, #20209, .T. ) ;
#7441 = ORIENTED_EDGE ( 'NONE', *, *, #7356, .T. ) ;
#7442 = EDGE_CURVE ( 'NONE', #860, #9208, #21154, .T. ) ;
#7443 = AXIS2_PLACEMENT_3D ( 'NONE', #17164, #8122, #15020 ) ;
#7444 = VERTEX_POINT ( 'NONE', #9962 ) ;
#7445 = ORIENTED_EDGE ( 'NONE', *, *, #12688, .T. ) ;
#7446 = ORIENTED_EDGE ( 'NONE', *, *, #21180, .F. ) ;
#7447 = VECTOR ( 'NONE', #4477, 999.9999999999998863 ) ;
#7448 = CARTESIAN_POINT ( 'NONE',  ( 157.4999999999998579, 55.73418700828869277, -45.00000000000000000 ) ) ;
#7449 = DIRECTION ( 'NONE',  ( 1.000000000000000000, 0.000000000000000000, 0.000000000000000000 ) ) ;
#7450 = FACE_OUTER_BOUND ( 'NONE', #18532, .T. ) ;
#7451 = MECHANICAL_DESIGN_GEOMETRIC_PRESENTATION_REPRESENTATION (  '', ( #14790 ), #17091 ) ;
#7452 = CARTESIAN_POINT ( 'NONE',  ( -82.62938906138147388, 134.8301624926916986, -15.44879298257729161 ) ) ;
#7453 = EDGE_CURVE ( 'NONE', #19895, #11442, #18720, .T. ) ;
#7454 = UNCERTAINTY_MEASURE_WITH_UNIT (LENGTH_MEASURE( 1.000000000000000082E-05 ), #5896, 'distance_accuracy_value', 'NONE');
#7455 = DIRECTION ( 'NONE',  ( -0.8916010070293283185, -0.4528218681383305855, 0.000000000000000000 ) ) ;
#7456 = CARTESIAN_POINT ( 'NONE',  ( -209.5875676835875083, 74.18578632021306873, 35.35260769160358052 ) ) ;
#7457 = CARTESIAN_POINT ( 'NONE',  ( -210.0000000000000853, -216.9546086794800317, 90.40281535134961644 ) ) ;
#7458 = CARTESIAN_POINT ( 'NONE',  ( -148.2538183076392215, 125.4301416103809288, -17.54546909480966121 ) ) ;
#7459 = CARTESIAN_POINT ( 'NONE',  ( 79.99999999999997158, 99.82480251742194355, -92.60160435377096633 ) ) ;
#7460 = CARTESIAN_POINT ( 'NONE',  ( 158.0000000000011369, 98.11412463215494029, 45.00000000000000000 ) ) ;
#7461 = CARTESIAN_POINT ( 'NONE',  ( 179.9999999999999147, -150.0000000000000284, 100.0000000000000142 ) ) ;
#7462 = PLANE ( 'NONE',  #18274 ) ;
#7463 = DIRECTION ( 'NONE',  ( 1.000000000000000000, 0.000000000000000000, 0.000000000000000000 ) ) ;
#7464 = VECTOR ( 'NONE', #26596, 1000.000000000000114 ) ;
#7465 = EDGE_CURVE ( 'NONE', #17680, #18077, #3343, .T. ) ;
#7466 = AXIS2_PLACEMENT_3D ( 'NONE', #18270, #7358, #27023 ) ;
#7467 = CARTESIAN_POINT ( 'NONE',  ( 217.4999999999996305, -5.589247009368136787, -100.0000000000000142 ) ) ;
#7468 = CARTESIAN_POINT ( 'NONE',  ( 116.3389527600916722, 113.0483370489294686, -100.0000000000000142 ) ) ;
#7469 = ADVANCED_BREP_SHAPE_REPRESENTATION ( '', ( #27918, #10637 ), #5568 ) ;
#7470 = DIRECTION ( 'NONE',  ( 0.000000000000000000, 0.000000000000000000, -1.000000000000000000 ) ) ;
#7471 = VECTOR ( 'NONE', #2959, 1000.000000000000000 ) ;
#7473 = ORIENTED_EDGE ( 'NONE', *, *, #12545, .F. ) ;
#7472 = ORIENTED_EDGE ( 'NONE', *, *, #4234, .T. ) ;
#7474 = VECTOR ( 'NONE', #3138, 999.9999999999998863 ) ;
#7475 = LINE ( 'NONE', #20818, #5609 ) ;
#7476 = ORIENTED_EDGE ( 'NONE', *, *, #25409, .F. ) ;
#7477 = VERTEX_POINT ( 'NONE', #8088 ) ;
#7478 = PLANE ( 'NONE',  #576 ) ;
#7479 = CARTESIAN_POINT ( 'NONE',  ( -81.45374247556539160, 136.3900883041769134, 15.17089325038065795 ) ) ;
#7480 = VERTEX_POINT ( 'NONE', #5925 ) ;
#7481 = VERTEX_POINT ( 'NONE', #23452 ) ;
#7482 = CARTESIAN_POINT ( 'NONE',  ( 158.0000000000003411, 173.8582498648732440, 45.00000000000000000 ) ) ;
#7483 = EDGE_CURVE ( 'NONE', #26789, #26868, #18065, .T. ) ;
#7484 = VECTOR ( 'NONE', #18367, 1000.000000000000000 ) ;
#7485 = CARTESIAN_POINT ( 'NONE',  ( 109.9999999999999289, -70.00000000000001421, 70.00000000000001421 ) ) ;
#7486 = EDGE_CURVE ( 'NONE', #2939, #15999, #25326, .T. ) ;
#7487 = VECTOR ( 'NONE', #21620, 1000.000000000000000 ) ;
#7488 = CARTESIAN_POINT ( 'NONE',  ( 232.4999999999996305, 83.06687458711267880, 36.86484227207694175 ) ) ;
#7489 = ADVANCED_FACE ( 'NONE', ( #2820 ), #20354, .F. ) ;
#7490 = CIRCLE ( 'NONE', #23537, 5.000000000000004441 ) ;
#7491 = DIRECTION ( 'NONE',  ( 0.8916010070298961976, -0.4528218681372121468, 0.000000000000000000 ) ) ;
#7492 = VECTOR ( 'NONE', #13885, 1000.000000000000000 ) ;
#7493 = FACE_OUTER_BOUND ( 'NONE', #4354, .T. ) ;
#7494 = CARTESIAN_POINT ( 'NONE',  ( 158.0000000000011369, 98.11412463215494029, 45.00000000000000000 ) ) ;
#7495 = CARTESIAN_POINT ( 'NONE',  ( -218.5620487852755218, 71.28382977987342883, -22.94473774457503978 ) ) ;
#7496 = CARTESIAN_POINT ( 'NONE',  ( 222.4999999999996021, 186.4134324495536248, -35.02193266779035952 ) ) ;
#7497 = DIRECTION ( 'NONE',  ( -0.8916010070297846202, 0.4528218681374320820, 0.000000000000000000 ) ) ;
#7498 = DIRECTION ( 'NONE',  ( 0.000000000000000000, 0.000000000000000000, -1.000000000000000000 ) ) ;
#7499 = LINE ( 'NONE', #25148, #15802 ) ;
#7500 = EDGE_LOOP ( 'NONE', ( #13699, #7828, #20749, #1184 ) ) ;
#7501 = VECTOR ( 'NONE', #26050, 1000.000000000000000 ) ;
#7502 = DIRECTION ( 'NONE',  ( 0.3897722486529259234, -0.9209112846414911902, 0.000000000000000000 ) ) ;
#7503 = VECTOR ( 'NONE', #17841, 1000.000000000000000 ) ;
#7504 = DIRECTION ( 'NONE',  ( 0.000000000000000000, -1.000000000000000000, -1.214306433183764966E-16 ) ) ;
#7505 = CARTESIAN_POINT ( 'NONE',  ( 11.56692809527929278, 215.3083398198040470, 45.00000000000000000 ) ) ;
#7506 = ORIENTED_EDGE ( 'NONE', *, *, #13099, .T. ) ;
#7507 = CARTESIAN_POINT ( 'NONE',  ( 45.16606905829554819, -21.98112499027946143, -0.2844719111299021108 ) ) ;
#7508 = VECTOR ( 'NONE', #15488, 1000.000000000000000 ) ;
#7509 = EDGE_LOOP ( 'NONE', ( #5210, #24995, #6584, #5103 ) ) ;
#7510 = CARTESIAN_POINT ( 'NONE',  ( 109.5756401947595862, 134.3783162857569664, 100.0000000000216573 ) ) ;
#7511 = CARTESIAN_POINT ( 'NONE',  ( 158.0000000000004263, 168.3346248423521274, -45.00000000000000000 ) ) ;
#7512 = ORIENTED_EDGE ( 'NONE', *, *, #546, .F. ) ;
#7513 = ADVANCED_FACE ( 'NONE', ( #23177 ), #5121, .T. ) ;
#7514 = VERTEX_POINT ( 'NONE', #10950 ) ;
#7515 = EDGE_CURVE ( 'NONE', #5835, #4162, #28027, .T. ) ;
#7516 = CARTESIAN_POINT ( 'NONE',  ( 222.4999999999996021, 194.4107529906318064, -62.90796922943941638 ) ) ;
#7517 = EDGE_CURVE ( 'NONE', #14722, #7676, #3907, .T. ) ;
#7518 = CARTESIAN_POINT ( 'NONE',  ( 157.9999999999996874, 271.1575001501400379, 45.00000000000000000 ) ) ;
#7519 = EDGE_CURVE ( 'NONE', #16964, #4623, #21578, .T. ) ;
#7520 = LINE ( 'NONE', #5349, #11899 ) ;
#7521 = VERTEX_POINT ( 'NONE', #21433 ) ;
#7522 = CARTESIAN_POINT ( 'NONE',  ( 79.99999999999994316, 80.00000000000001421, 100.0000000000000142 ) ) ;
#7523 = ORIENTED_EDGE ( 'NONE', *, *, #17446, .T. ) ;
#7524 = VECTOR ( 'NONE', #24439, 1000.000000000000000 ) ;
#7525 = DIRECTION ( 'NONE',  ( -0.000000000000000000, -0.000000000000000000, -1.000000000000000000 ) ) ;
#7526 = VECTOR ( 'NONE', #2619, 1000.000000000000000 ) ;
#7527 = DIRECTION ( 'NONE',  ( -0.000000000000000000, -0.000000000000000000, -1.000000000000000000 ) ) ;
#7528 = DIRECTION ( 'NONE',  ( -0.4767408570798813972, 0.8790438869537404720, 0.000000000000000000 ) ) ;
#7529 = CARTESIAN_POINT ( 'NONE',  ( -7.291805129867194424, 132.9340346030435001, -15.80620534190248527 ) ) ;
#7530 = AXIS2_PLACEMENT_3D ( 'NONE', #19040, #27789, #21765 ) ;
#7531 = CARTESIAN_POINT ( 'NONE',  ( -210.0000000000000568, -150.0000000000000853, -99.99999999999995737 ) ) ;
#7532 = DIRECTION ( 'NONE',  ( 1.000000000000000000, 0.000000000000000000, 0.000000000000000000 ) ) ;
#7533 = CARTESIAN_POINT ( 'NONE',  ( 162.7359358511135952, 208.5633933773887350, -140.4786076439499709 ) ) ;
#7534 = VERTEX_POINT ( 'NONE', #21726 ) ;
#7535 = CARTESIAN_POINT ( 'NONE',  ( 65.00000000000000000, -150.0000000000000568, -75.99999999999998579 ) ) ;
#7536 = FACE_OUTER_BOUND ( 'NONE', #12105, .T. ) ;
#7537 = CARTESIAN_POINT ( 'NONE',  ( 222.4999999999996021, 194.4107529906318064, 58.31593845887894645 ) ) ;
#7538 = ORIENTED_EDGE ( 'NONE', *, *, #15430, .F. ) ;
#7539 = LINE ( 'NONE', #18587, #2230 ) ;
#7540 = ORIENTED_EDGE ( 'NONE', *, *, #13135, .F. ) ;
#7541 = LINE ( 'NONE', #9968, #13473 ) ;
#7542 = PLANE ( 'NONE',  #10557 ) ;
#7543 = LINE ( 'NONE', #25476, #19037 ) ;
#7544 = ORIENTED_EDGE ( 'NONE', *, *, #13363, .T. ) ;
#7545 = DIRECTION ( 'NONE',  ( 1.321694076934710155E-16, -1.000000000000000000, 0.000000000000000000 ) ) ;
#7546 = CARTESIAN_POINT ( 'NONE',  ( 157.4999999999998579, 120.9389372034718093, 45.00000000000000000 ) ) ;
#7547 = ORIENTED_EDGE ( 'NONE', *, *, #18693, .T. ) ;
#7548 = TOROIDAL_SURFACE ( 'NONE', #26793, 21.49999999999998224, 1.000000000000000000 ) ;
#7549 = EDGE_CURVE ( 'NONE', #19026, #11671, #16987, .T. ) ;
#7550 = ADVANCED_FACE ( 'NONE', ( #2036 ), #8369, .F. ) ;
#7551 = DIRECTION ( 'NONE',  ( 0.000000000000000000, 0.000000000000000000, 1.000000000000000000 ) ) ;
#7552 = CARTESIAN_POINT ( 'NONE',  ( 102.7211906516483424, 244.5533218984080293, 17.51413272308122160 ) ) ;
#7553 = ORIENTED_EDGE ( 'NONE', *, *, #1360, .T. ) ;
#7554 = VECTOR ( 'NONE', #6494, 1000.000000000000000 ) ;
#7555 = ORIENTED_EDGE ( 'NONE', *, *, #22019, .F. ) ;
#7556 = EDGE_CURVE ( 'NONE', #15387, #21202, #1890, .T. ) ;
#7557 = CARTESIAN_POINT ( 'NONE',  ( 65.00000000000000000, -150.0000000000000568, -64.00000000000000000 ) ) ;
#7558 = EDGE_LOOP ( 'NONE', ( #26937, #19974, #4102, #19024, #21588, #15542, #2364, #5798 ) ) ;
#7559 = ADVANCED_FACE ( 'NONE', ( #23735 ), #19760, .F. ) ;
#7560 = VERTEX_POINT ( 'NONE', #1749 ) ;
#7561 = ORIENTED_EDGE ( 'NONE', *, *, #17554, .F. ) ;
#7562 = B_SPLINE_CURVE_WITH_KNOTS ( 'NONE', 3,
 ( #15911, #675, #22791, #23069, #811, #16465, #14173, #3374, #1227, #5395, #12018, #3090, #20343, #9440, #5256, #947, #14310, #18340, #22926, #20764, #26950, #16332 ),
 .UNSPECIFIED., .F., .F.,
 ( 4, 2, 2, 2, 2, 2, 2, 2, 2, 2, 4 ),
 ( 0.000000000000000000, 0.06250000000000000000, 0.1250000000000000000, 0.1875000000000000000, 0.2500000000000000000, 0.3750000000000000000, 0.5000000000000000000, 0.6250000000000000000, 0.7500000000000000000, 0.8750000000000001110, 1.000000000000000000 ),
 .UNSPECIFIED. ) ;
#7563 = CARTESIAN_POINT ( 'NONE',  ( 109.9999999999999005, 260.0000000000000000, 45.00000000000000000 ) ) ;
#7564 = DIRECTION ( 'NONE',  ( 1.000000000000000000, 0.000000000000000000, 0.000000000000000000 ) ) ;
#7565 = CARTESIAN_POINT ( 'NONE',  ( 158.0000000000001990, 188.3976249024084666, -45.00000000000000000 ) ) ;
#7566 = AXIS2_PLACEMENT_3D ( 'NONE', #26302, #24021, #13388 ) ;
#7567 = CARTESIAN_POINT ( 'NONE',  ( -221.3650667873343139, -91.18033988749901653, 19.29759039828519818 ) ) ;
#7568 = DIRECTION ( 'NONE',  ( -0.000000000000000000, -0.000000000000000000, -1.000000000000000000 ) ) ;
#7569 = PLANE ( 'NONE',  #21234 ) ;
#7570 = LINE ( 'NONE', #9858, #10865 ) ;
#7571 = CIRCLE ( 'NONE', #10761, 562.1290781602207289 ) ;
#7572 = CARTESIAN_POINT ( 'NONE',  ( 158.0000000000015348, 60.49599951954928656, -45.00000000000000000 ) ) ;
#7573 = CARTESIAN_POINT ( 'NONE',  ( 111.9999999999999289, 218.9999999999996874, -45.00000000000000000 ) ) ;
#7574 = CARTESIAN_POINT ( 'NONE',  ( 0.000000000000000000, 330.0000000000000000, 100.0000000000000142 ) ) ;
#7575 = VERTEX_POINT ( 'NONE', #25740 ) ;
#7576 = CARTESIAN_POINT ( 'NONE',  ( 99.17397288323584803, 242.2128526578931371, -12.79873440004189966 ) ) ;
#7577 = CARTESIAN_POINT ( 'NONE',  ( 23.19384040928324708, 86.94809229719507471, 99.18534753508888002 ) ) ;
#7578 = DIRECTION ( 'NONE',  ( 0.8660254037844432595, 0.4999999999999919509, -0.000000000000000000 ) ) ;
#7579 = EDGE_LOOP ( 'NONE', ( #25051, #8485, #26970, #15613 ) ) ;
#7580 = EDGE_CURVE ( 'NONE', #5346, #19329, #6066, .T. ) ;
#7581 = DIRECTION ( 'NONE',  ( 1.000000000000000000, 0.000000000000000000, 0.000000000000000000 ) ) ;
#7582 = EDGE_LOOP ( 'NONE', ( #26944, #13920, #19726, #2572, #22514, #27301 ) ) ;
#7583 = CIRCLE ( 'NONE', #23623, 30.00000000000000000 ) ;
#7584 = AXIS2_PLACEMENT_3D ( 'NONE', #4535, #10880, #26090 ) ;
#7585 = VECTOR ( 'NONE', #10205, 1000.000000000000000 ) ;
#7586 = ORIENTED_EDGE ( 'NONE', *, *, #2428, .T. ) ;
#7587 = EDGE_LOOP ( 'NONE', ( #27520, #2778, #27653, #10159, #21037, #14648 ) ) ;
#7588 = VERTEX_POINT ( 'NONE', #8515 ) ;
#7589 = AXIS2_PLACEMENT_3D ( 'NONE', #12281, #24919, #22903 ) ;
#7590 = VERTEX_POINT ( 'NONE', #4189 ) ;
#7591 = CARTESIAN_POINT ( 'NONE',  ( -142.4951090877017634, 127.4563655094269023, 16.43271896145171240 ) ) ;
#7592 = CARTESIAN_POINT ( 'NONE',  ( -230.8916957670046486, 130.8330661503598833, 15.00000000000000000 ) ) ;
#7593 = CARTESIAN_POINT ( 'NONE',  ( -211.9731542214773583, -220.0000000000000853, -93.39625318057545655 ) ) ;
#7594 = ADVANCED_FACE ( 'NONE', ( #15274 ), #10527, .F. ) ;
#7595 = CARTESIAN_POINT ( 'NONE',  ( 157.4999999999998579, 53.22631200078164682, 45.00000000000000000 ) ) ;
#7596 = CARTESIAN_POINT ( 'NONE',  ( -11.61564047653929599, 131.4612359469146838, 14.74843121655267275 ) ) ;
#7597 = DIRECTION ( 'NONE',  ( -9.345788444546305817E-17, 0.7071067811865494601, 0.7071067811865456854 ) ) ;
#7598 = CARTESIAN_POINT ( 'NONE',  ( 157.4999999999998579, 78.30506207585207790, 45.00000000000000000 ) ) ;
#7599 = CARTESIAN_POINT ( 'NONE',  ( 58.09044720719344213, 216.7965004116395562, 45.00000000000000000 ) ) ;
#7600 = CARTESIAN_POINT ( 'NONE',  ( 158.0000000000012506, 88.08262460212675649, 45.00000000000000000 ) ) ;
#7601 = CARTESIAN_POINT ( 'NONE',  ( 157.4999999999998579, 73.28931206083800021, 45.00000000000000000 ) ) ;
#7602 = DIRECTION ( 'NONE',  ( 0.000000000000000000, 0.000000000000000000, -1.000000000000000000 ) ) ;
#7603 = CIRCLE ( 'NONE', #1168, 6.025000000000002132 ) ;
#7604 = CARTESIAN_POINT ( 'NONE',  ( 156.4999999999998579, 220.0000000000000284, -100.0000000000000142 ) ) ;
#7605 = CIRCLE ( 'NONE', #6212, 5.999999999999991118 ) ;
#7606 = ORIENTED_EDGE ( 'NONE', *, *, #17289, .T. ) ;
#7607 = ADVANCED_FACE ( 'NONE', ( #14850 ), #15413, .F. ) ;
#7608 = CARTESIAN_POINT ( 'NONE',  ( 158.0000000000012221, 88.59049960963380954, 45.00000000000000000 ) ) ;
#7609 = CARTESIAN_POINT ( 'NONE',  ( 79.99999999999991473, 80.00000000000001421, -100.0000000000000142 ) ) ;
#7610 = DIRECTION ( 'NONE',  ( 0.000000000000000000, 0.000000000000000000, -1.000000000000000000 ) ) ;
#7611 = VECTOR ( 'NONE', #9200, 1000.000000000000114 ) ;
#7613 = ORIENTED_EDGE ( 'NONE', *, *, #6756, .T. ) ;
#7612 = VERTEX_POINT ( 'NONE', #25887 ) ;
#7614 = EDGE_CURVE ( 'NONE', #4345, #24637, #24167, .T. ) ;
#7615 = LINE ( 'NONE', #10045, #10208 ) ;
#7616 = ORIENTED_EDGE ( 'NONE', *, *, #25278, .T. ) ;
#7617 = EDGE_LOOP ( 'NONE', ( #923, #16798, #3735, #7752 ) ) ;
#7618 = VERTEX_POINT ( 'NONE', #17409 ) ;
#7619 = AXIS2_PLACEMENT_3D ( 'NONE', #27597, #3476, #23984 ) ;
#7620 = VERTEX_POINT ( 'NONE', #26168 ) ;
#7621 = CARTESIAN_POINT ( 'NONE',  ( 157.4999999999997158, 261.3799376238655441, 45.00000000000000000 ) ) ;
#7622 = AXIS2_PLACEMENT_3D ( 'NONE', #5096, #20472, #20038 ) ;
#7623 = DIRECTION ( 'NONE',  ( -9.251858538542974046E-17, -1.214306433183764966E-16, 1.000000000000000000 ) ) ;
#7624 = EDGE_CURVE ( 'NONE', #12356, #16763, #6492, .T. ) ;
#7625 = EDGE_CURVE ( 'NONE', #12468, #2948, #11050, .T. ) ;
#7626 = LINE ( 'NONE', #9643, #4098 ) ;
#7627 = PLANE ( 'NONE',  #10264 ) ;
#7628 = CARTESIAN_POINT ( 'NONE',  ( -123.8208147886770121, 198.8605305197760913, -15.00000000000000000 ) ) ;
#7629 = DIRECTION ( 'NONE',  ( -0.000000000000000000, -0.000000000000000000, -1.000000000000000000 ) ) ;
#7630 = DIRECTION ( 'NONE',  ( 0.4528218681374520105, 0.8916010070297746282, -0.000000000000000000 ) ) ;
#7631 = CARTESIAN_POINT ( 'NONE',  ( 134.9999999999998579, 268.4896896257338881, 84.99999999999995737 ) ) ;
#7632 = ADVANCED_FACE ( 'NONE', ( #19284, #19571 ), #1613, .F. ) ;
#7633 = CARTESIAN_POINT ( 'NONE',  ( 111.8061829044033004, 200.9721503227722508, -148.4939404368777218 ) ) ;
#7634 = CARTESIAN_POINT ( 'NONE',  ( -279.3160071107327553, -83.68033988749907337, 0.000000000000000000 ) ) ;
#7635 = FACE_BOUND ( 'NONE', #12245, .T. ) ;
#7636 = DIRECTION ( 'NONE',  ( 0.000000000000000000, 0.000000000000000000, 1.000000000000000000 ) ) ;
#7637 = VERTEX_POINT ( 'NONE', #15127 ) ;
#7639 = EDGE_CURVE ( 'NONE', #27397, #19273, #15551, .T. ) ;
#7638 = AXIS2_PLACEMENT_3D ( 'NONE', #4665, #17895, #6968 ) ;
#7640 = DIRECTION ( 'NONE',  ( -0.000000000000000000, 0.000000000000000000, -1.000000000000000000 ) ) ;
#7641 = EDGE_CURVE ( 'NONE', #23548, #20178, #2316, .T. ) ;
#7642 = CARTESIAN_POINT ( 'NONE',  ( -240.4233474261503716, 71.57180907113834678, 14.67903078147715235 ) ) ;
#7643 = LINE ( 'NONE', #12104, #24582 ) ;
#7644 = ORIENTED_EDGE ( 'NONE', *, *, #436, .F. ) ;
#7645 = DIRECTION ( 'NONE',  ( -1.387778780781445429E-16, 1.387778780781445429E-16, 1.000000000000000000 ) ) ;
#7646 = EDGE_CURVE ( 'NONE', #7612, #7786, #26645, .T. ) ;
#7647 = VECTOR ( 'NONE', #16335, 1000.000000000000000 ) ;
#7648 = ORIENTED_EDGE ( 'NONE', *, *, #10080, .T. ) ;
#7649 = DIRECTION ( 'NONE',  ( 0.7071067811867438602, 0.000000000000000000, -0.7071067811863512853 ) ) ;
#7650 = DIRECTION ( 'NONE',  ( -0.8916010070297751833, -0.4528218681374507892, 0.000000000000000000 ) ) ;
#7651 = ORIENTED_EDGE ( 'NONE', *, *, #8934, .T. ) ;
#7652 = VERTEX_POINT ( 'NONE', #6768 ) ;
#7653 = CARTESIAN_POINT ( 'NONE',  ( 157.9999999999996589, 274.1732501651540588, 45.00000000000000000 ) ) ;
#7654 = CARTESIAN_POINT ( 'NONE',  ( 217.4999999999996305, 258.6181251126050711, 6.025000000000016342 ) ) ;
#7655 = CARTESIAN_POINT ( 'NONE',  ( 157.4999999999998579, 146.0176872785422404, 45.00000000000000000 ) ) ;
#7657 = EDGE_CURVE ( 'NONE', #19790, #7652, #9514, .T. ) ;
#7656 = ORIENTED_EDGE ( 'NONE', *, *, #14413, .T. ) ;
#7658 = DIRECTION ( 'NONE',  ( 1.000000000000000000, 0.000000000000000000, 0.000000000000000000 ) ) ;
#7659 = VERTEX_POINT ( 'NONE', #17835 ) ;
#7660 = VECTOR ( 'NONE', #12294, 1000.000000000000114 ) ;
#7661 = DIRECTION ( 'NONE',  ( 1.321694076934710155E-16, -1.000000000000000000, 0.000000000000000000 ) ) ;
#7662 = PLANE ( 'NONE',  #14034 ) ;
#7663 = CARTESIAN_POINT ( 'NONE',  ( 157.4999999999998579, 161.0649373235845019, 45.00000000000000000 ) ) ;
#7664 = DIRECTION ( 'NONE',  ( 0.000000000000000000, -1.000000000000000000, 0.000000000000000000 ) ) ;
#7665 = CARTESIAN_POINT ( 'NONE',  ( 157.4999999999998579, 153.5413123010633853, 45.00000000000000000 ) ) ;
#7666 = LINE ( 'NONE', #16432, #12435 ) ;
#7667 = CARTESIAN_POINT ( 'NONE',  ( 109.9999999999999289, 110.0000000000000142, -45.00000000000000000 ) ) ;
#7668 = ORIENTED_EDGE ( 'NONE', *, *, #8934, .F. ) ;
#7669 = CARTESIAN_POINT ( 'NONE',  ( 432.4999999999996589, -5.589247009368158103, 75.99342076785332267 ) ) ;
#7670 = CARTESIAN_POINT ( 'NONE',  ( 177.1897033089359184, 197.3087408678716770, 45.00000000000000000 ) ) ;
#7671 = CARTESIAN_POINT ( 'NONE',  ( 158.0000000000010800, 101.1298746471690038, 45.00000000000000000 ) ) ;
#7672 = ORIENTED_EDGE ( 'NONE', *, *, #1960, .T. ) ;
#7673 = EDGE_CURVE ( 'NONE', #7009, #25157, #15985, .T. ) ;
#7674 = CARTESIAN_POINT ( 'NONE',  ( -236.3091765109048197, 68.24607436519742976, 5.736201002603997345 ) ) ;
#7675 = EDGE_CURVE ( 'NONE', #4902, #8063, #7357, .T. ) ;
#7676 = VERTEX_POINT ( 'NONE', #8935 ) ;
#7677 = DIRECTION ( 'NONE',  ( -0.8660254037844363761, 0.5000000000000041078, -0.000000000000000000 ) ) ;
#7678 = CARTESIAN_POINT ( 'NONE',  ( 134.9999999999998579, 467.1080826427131001, -145.0000000000000000 ) ) ;
#7679 = CARTESIAN_POINT ( 'NONE',  ( 136.5616572741750474, 249.9618117005867077, -139.1934629298939115 ) ) ;
#7680 = VERTEX_POINT ( 'NONE', #26738 ) ;
#7681 = CARTESIAN_POINT ( 'NONE',  ( -160.0000000000000284, 59.99999999999994316, 45.00000000000000000 ) ) ;
#7682 = FILL_AREA_STYLE_COLOUR ( '', #3754 ) ;
#7683 = ORIENTED_EDGE ( 'NONE', *, *, #11045, .F. ) ;
#7684 = AXIS2_PLACEMENT_3D ( 'NONE', #11669, #20405, #18258 ) ;
#7685 = CLOSED_SHELL ( 'NONE', ( #27662, #5859, #10923, #13213, #638, #25140, #12744, #862, #18950, #19519, #7276, #21054, #26875, #12538, #12366, #2085, #16790, #21383, #15295, #4293, #3427, #10099, #7950, #11235, #9891, #10487, #18643, #7632, #4858, #26174, #23715, #1696, #14081, #13988, #21540, #15788, #18376, #21415, #23268, #16251, #4534, #4708, #3274, #7559 ) ) ;
#7686 = DIRECTION ( 'NONE',  ( 1.541976423090495387E-16, -1.000000000000000000, 0.000000000000000000 ) ) ;
#7687 = LINE ( 'NONE', #23052, #22297 ) ;
#7688 = VERTEX_POINT ( 'NONE', #11537 ) ;
#7689 = ORIENTED_EDGE ( 'NONE', *, *, #10328, .T. ) ;
#7690 = CARTESIAN_POINT ( 'NONE',  ( 157.9999999999996874, 266.6496251426330559, 45.00000000000000000 ) ) ;
#7691 = VERTEX_POINT ( 'NONE', #11385 ) ;
#7692 = EDGE_CURVE ( 'NONE', #24469, #17639, #20130, .T. ) ;
#7693 = ORIENTED_EDGE ( 'NONE', *, *, #11001, .T. ) ;
#7694 = ORIENTED_EDGE ( 'NONE', *, *, #8179, .T. ) ;
#7695 = CARTESIAN_POINT ( 'NONE',  ( 109.8079904625031276, 257.1776683528518106, 40.10892953524286497 ) ) ;
#7696 = AXIS2_PLACEMENT_3D ( 'NONE', #8647, #21862, #17404 ) ;
#7697 = EDGE_CURVE ( 'NONE', #24318, #8004, #17482, .T. ) ;
#7698 = CARTESIAN_POINT ( 'NONE',  ( -215.4886702565632106, 139.8420026707766226, 12.99999999999999822 ) ) ;
#7699 = DIRECTION ( 'NONE',  ( -0.000000000000000000, -0.000000000000000000, -1.000000000000000000 ) ) ;
#7700 = VECTOR ( 'NONE', #18641, 1000.000000000000114 ) ;
#7701 = LINE ( 'NONE', #27359, #3223 ) ;
#7702 = CARTESIAN_POINT ( 'NONE',  ( 157.9999999999999147, 213.9842499849850697, 45.00000000000000000 ) ) ;
#7703 = DIRECTION ( 'NONE',  ( -0.8916010070294301260, -0.4528218681381301347, 0.000000000000000000 ) ) ;
#7704 = DIRECTION ( 'NONE',  ( 1.000000000000000000, 0.000000000000000000, 0.000000000000000000 ) ) ;
#7705 = EDGE_CURVE ( 'NONE', #26626, #20330, #27022, .T. ) ;
#7706 = CARTESIAN_POINT ( 'NONE',  ( 158.0000000000005400, 155.7952498048169048, -45.00000000000000000 ) ) ;
#7707 = CARTESIAN_POINT ( 'NONE',  ( 0.1700960744404878267, -1.249999999999999112, -7.344776659773097016 ) ) ;
#7708 = DIRECTION ( 'NONE',  ( -0.8660254037844431485, -0.4999999999999922284, 0.000000000000000000 ) ) ;
#7709 = ORIENTED_EDGE ( 'NONE', *, *, #27755, .T. ) ;
#7710 = ADVANCED_FACE ( 'NONE', ( #16124 ), #21853, .T. ) ;
#7711 = ADVANCED_FACE ( 'NONE', ( #5188 ), #12380, .T. ) ;
#7712 = PLANE ( 'NONE',  #15593 ) ;
#7713 = DIRECTION ( 'NONE',  ( 0.4528218681378110011, -0.8916010070295922185, 0.000000000000000000 ) ) ;
#7714 = CARTESIAN_POINT ( 'NONE',  ( -221.3650667873343139, -91.18033988749901653, -19.29759039828519818 ) ) ;
#7715 = DIRECTION ( 'NONE',  ( -1.000000000000000000, 0.000000000000000000, 0.000000000000000000 ) ) ;
#7716 = ORIENTED_EDGE ( 'NONE', *, *, #701, .F. ) ;
#7717 = DIRECTION ( 'NONE',  ( -0.000000000000000000, -0.000000000000000000, -1.000000000000000000 ) ) ;
#7718 = ORIENTED_EDGE ( 'NONE', *, *, #22566, .T. ) ;
#7719 = DIRECTION ( 'NONE',  ( 0.000000000000000000, -1.000000000000000000, -9.486769009248162565E-17 ) ) ;
#7720 = AXIS2_PLACEMENT_3D ( 'NONE', #4084, #10706, #6803 ) ;
#7721 = ORIENTED_EDGE ( 'NONE', *, *, #19399, .T. ) ;
#7722 = ORIENTED_EDGE ( 'NONE', *, *, #3717, .F. ) ;
#7723 = ORIENTED_EDGE ( 'NONE', *, *, #448, .F. ) ;
#7724 = ORIENTED_EDGE ( 'NONE', *, *, #1867, .F. ) ;
#7725 = EDGE_LOOP ( 'NONE', ( #20077, #6847, #6187, #26324 ) ) ;
#7726 = PLANE ( 'NONE',  #20515 ) ;
#7727 = DIRECTION ( 'NONE',  ( 1.000000000000000000, 0.000000000000000000, 0.000000000000000000 ) ) ;
#7728 = CARTESIAN_POINT ( 'NONE',  ( -212.2419371577845197, -220.0000000000000568, -94.58889440303579477 ) ) ;
#7729 = CIRCLE ( 'NONE', #14220, 19.07743405327024888 ) ;
#7730 = CARTESIAN_POINT ( 'NONE',  ( -92.67942046851547389, 134.7159439475681779, -15.46877993217822400 ) ) ;
#7731 = CARTESIAN_POINT ( 'NONE',  ( -260.0000000000001137, -157.0000000000000284, -59.99999999999986500 ) ) ;
#7732 = CARTESIAN_POINT ( 'NONE',  ( -180.0000000000000284, -50.00000000000004263, 110.0000000000000284 ) ) ;
#7733 = EDGE_CURVE ( 'NONE', #9639, #14325, #18967, .T. ) ;
#7734 = CARTESIAN_POINT ( 'NONE',  ( -160.8326600028555902, 120.2355194873575073, -21.37420696376537776 ) ) ;
#7735 = CARTESIAN_POINT ( 'NONE',  ( 134.9999999999998579, 250.0000000000000568, -138.9999999999999432 ) ) ;
#7736 = AXIS2_PLACEMENT_3D ( 'NONE', #18929, #5850, #14622 ) ;
#7737 = LINE ( 'NONE', #25113, #16743 ) ;
#7738 = FACE_OUTER_BOUND ( 'NONE', #4787, .T. ) ;
#7739 = LINE ( 'NONE', #9760, #11847 ) ;
#7740 = DIRECTION ( 'NONE',  ( 0.000000000000000000, -1.000000000000000000, -0.000000000000000000 ) ) ;
#7741 = ORIENTED_EDGE ( 'NONE', *, *, #3838, .F. ) ;
#7742 = EDGE_CURVE ( 'NONE', #8983, #23817, #20555, .T. ) ;
#7743 = CARTESIAN_POINT ( 'NONE',  ( -201.8712871270307971, 91.53752412319902021, -28.77272332722132120 ) ) ;
#7744 = DIRECTION ( 'NONE',  ( 0.000000000000000000, -1.000000000000000000, 0.000000000000000000 ) ) ;
#7745 = LINE ( 'NONE', #14359, #15758 ) ;
#7747 = ORIENTED_EDGE ( 'NONE', *, *, #14984, .F. ) ;
#7746 = ORIENTED_EDGE ( 'NONE', *, *, #2527, .T. ) ;
#7748 = EDGE_CURVE ( 'NONE', #7612, #1333, #27122, .T. ) ;
#7749 = AXIS2_PLACEMENT_3D ( 'NONE', #10489, #4302, #28276 ) ;
#7750 = PLANE ( 'NONE',  #5166 ) ;
#7751 = ORIENTED_EDGE ( 'NONE', *, *, #18188, .T. ) ;
#7752 = ORIENTED_EDGE ( 'NONE', *, *, #12448, .T. ) ;
#7753 = ORIENTED_EDGE ( 'NONE', *, *, #27498, .F. ) ;
#7754 = AXIS2_PLACEMENT_3D ( 'NONE', #18821, #14524, #1716 ) ;
#7755 = VECTOR ( 'NONE', #14979, 1000.000000000000000 ) ;
#7756 = ORIENTED_EDGE ( 'NONE', *, *, #23297, .F. ) ;
#7757 = ORIENTED_EDGE ( 'NONE', *, *, #27019, .F. ) ;
#7758 = DIRECTION ( 'NONE',  ( -1.000000000000000000, 0.000000000000000000, 0.000000000000000000 ) ) ;
#7759 = EDGE_CURVE ( 'NONE', #27147, #23757, #27294, .T. ) ;
#7760 = CARTESIAN_POINT ( 'NONE',  ( 118.0294372515226939, 235.5563491861037164, -45.00000000000000000 ) ) ;
#7761 = AXIS2_PLACEMENT_3D ( 'NONE', #20264, #26876, #11372 ) ;
#7762 = DIRECTION ( 'NONE',  ( 0.8916010070298455714, -0.4528218681373120669, 0.000000000000000000 ) ) ;
#7763 = CARTESIAN_POINT ( 'NONE',  ( 109.9696209020443973, 258.3904084527665077, -43.60594690666008688 ) ) ;
#7764 = CARTESIAN_POINT ( 'NONE',  ( 65.00000000000000000, -170.0000000000000568, 64.00000000000004263 ) ) ;
#7765 = EDGE_CURVE ( 'NONE', #8109, #8669, #20694, .T. ) ;
#7766 = AXIS2_PLACEMENT_3D ( 'NONE', #6533, #4646, #15739 ) ;
#7767 = CARTESIAN_POINT ( 'NONE',  ( 158.0000000000017053, 43.44874947450702507, 45.00000000000000000 ) ) ;
#7768 = DIRECTION ( 'NONE',  ( -1.000000000000000000, -1.321694076934710155E-16, 0.000000000000000000 ) ) ;
#7769 = CARTESIAN_POINT ( 'NONE',  ( -207.4994891700685002, 75.60264349980251097, -44.78213549412046746 ) ) ;
#7770 = TOROIDAL_SURFACE ( 'NONE', #878, -538.1631314933625845, 562.1290781602207289 ) ;
#7771 = CARTESIAN_POINT ( 'NONE',  ( -189.5231184314577604, 157.6231267382823091, 15.00000000000000000 ) ) ;
#7772 = CARTESIAN_POINT ( 'NONE',  ( -270.1025481742786951, -91.18033988749901653, -14.95564396479129243 ) ) ;
#7773 = FACE_OUTER_BOUND ( 'NONE', #13844, .T. ) ;
#7774 = VERTEX_POINT ( 'NONE', #22997 ) ;
#7775 = DIRECTION ( 'NONE',  ( 0.000000000000000000, 0.000000000000000000, -1.000000000000000000 ) ) ;
#7776 = ADVANCED_FACE ( 'NONE', ( #10212 ), #25289, .T. ) ;
#7777 = ADVANCED_FACE ( 'NONE', ( #880 ), #18409, .F. ) ;
#7778 = LINE ( 'NONE', #23004, #14478 ) ;
#7779 = VERTEX_POINT ( 'NONE', #3163 ) ;
#7780 = ORIENTED_EDGE ( 'NONE', *, *, #13847, .F. ) ;
#7781 = ORIENTED_EDGE ( 'NONE', *, *, #15351, .T. ) ;
#7782 = LINE ( 'NONE', #23430, #1926 ) ;
#7783 = AXIS2_PLACEMENT_3D ( 'NONE', #23948, #15048, #26230 ) ;
#7784 = CARTESIAN_POINT ( 'NONE',  ( 1.250275373174978055, 1.249999999999999556, 7.480737022738205511 ) ) ;
#7785 = ORIENTED_EDGE ( 'NONE', *, *, #10298, .F. ) ;
#7787 = EDGE_CURVE ( 'NONE', #19329, #21631, #24376, .T. ) ;
#7786 = VERTEX_POINT ( 'NONE', #23281 ) ;
#7788 = CARTESIAN_POINT ( 'NONE',  ( 87.74278500246884960, 111.0010834413659921, -71.13281249983540988 ) ) ;
#7789 = AXIS2_PLACEMENT_3D ( 'NONE', #7433, #20358, #11895 ) ;
#7790 = EDGE_CURVE ( 'NONE', #6688, #19256, #16539, .T. ) ;
#7791 = CARTESIAN_POINT ( 'NONE',  ( 107.9379653822511216, 247.3366651132932077, 33.97036151511563418 ) ) ;
#7792 = DIRECTION ( 'NONE',  ( -0.000000000000000000, -0.000000000000000000, 1.000000000000000000 ) ) ;
#7793 = ORIENTED_EDGE ( 'NONE', *, *, #20537, .F. ) ;
#7794 = CARTESIAN_POINT ( 'NONE',  ( -229.4141265690028604, 89.10432210626537142, 15.37309836091423954 ) ) ;
#7795 = ORIENTED_EDGE ( 'NONE', *, *, #12508, .F. ) ;
#7796 = DIRECTION ( 'NONE',  ( 1.000000000000000000, 1.321694076934710155E-16, 0.000000000000000000 ) ) ;
#7797 = PLANE ( 'NONE',  #20919 ) ;
#7798 = ADVANCED_FACE ( 'NONE', ( #25431 ), #1435, .F. ) ;
#7799 = DIRECTION ( 'NONE',  ( 0.8660254037844394848, 0.4999999999999985012, -0.000000000000000000 ) ) ;
#7800 = CARTESIAN_POINT ( 'NONE',  ( 157.9999999999997726, 246.5866250825770294, 45.00000000000000000 ) ) ;
#7801 = PLANE ( 'NONE',  #20068 ) ;
#7802 = DIRECTION ( 'NONE',  ( -0.000000000000000000, 0.000000000000000000, 1.000000000000000000 ) ) ;
#7803 = CARTESIAN_POINT ( 'NONE',  ( -183.1437745737416947, 107.7727709130676743, -31.77045322972226060 ) ) ;
#7804 = ORIENTED_EDGE ( 'NONE', *, *, #5878, .F. ) ;
#7805 = AXIS2_PLACEMENT_3D ( 'NONE', #22071, #9002, #19768 ) ;
#7806 = DIRECTION ( 'NONE',  ( 1.000000000000000000, -0.000000000000000000, -0.000000000000000000 ) ) ;
#7807 = DIRECTION ( 'NONE',  ( -0.9784193629480828491, -0.2066290158914464437, 0.000000000000000000 ) ) ;
#7808 = CARTESIAN_POINT ( 'NONE',  ( 157.9999999999998579, 223.5078750075070104, 45.00000000000000000 ) ) ;
#7809 = CARTESIAN_POINT ( 'NONE',  ( -12.24491960465745599, 75.97823757117562593, 100.0000000000000000 ) ) ;
#7810 = ORIENTED_EDGE ( 'NONE', *, *, #10060, .F. ) ;
#7811 = DIRECTION ( 'NONE',  ( 0.000000000000000000, 1.000000000000000000, 0.000000000000000000 ) ) ;
#7812 = AXIS2_PLACEMENT_3D ( 'NONE', #24129, #25985, #17652 ) ;
#7813 = ORIENTED_EDGE ( 'NONE', *, *, #20861, .F. ) ;
#7814 = CARTESIAN_POINT ( 'NONE',  ( 157.4999999999997158, 258.8720626163585621, 45.00000000000000000 ) ) ;
#7815 = LINE ( 'NONE', #11857, #8285 ) ;
#7816 = DIRECTION ( 'NONE',  ( 0.8916010070295207202, -0.4528218681379515553, 0.000000000000000000 ) ) ;
#7817 = EDGE_LOOP ( 'NONE', ( #24741, #22368, #6778, #19856 ) ) ;
#7818 = CARTESIAN_POINT ( 'NONE',  ( 157.4999999999998579, 58.24206201579573872, 45.00000000000000000 ) ) ;
#7819 = DIRECTION ( 'NONE',  ( -1.000000000000000000, -2.602085213965211135E-16, 0.000000000000000000 ) ) ;
#7820 = ORIENTED_EDGE ( 'NONE', *, *, #1800, .T. ) ;
#7821 = CARTESIAN_POINT ( 'NONE',  ( 158.0000000000016200, 50.97237449702815582, 45.00000000000000000 ) ) ;
#7822 = CARTESIAN_POINT ( 'NONE',  ( 158.0000000000011084, 100.6219996396619791, 45.00000000000000000 ) ) ;
#7823 = ORIENTED_EDGE ( 'NONE', *, *, #26911, .F. ) ;
#7824 = ORIENTED_EDGE ( 'NONE', *, *, #17747, .T. ) ;
#7825 = FACE_OUTER_BOUND ( 'NONE', #5930, .T. ) ;
#7826 = VERTEX_POINT ( 'NONE', #1158 ) ;
#7827 = VECTOR ( 'NONE', #4078, 1000.000000000000000 ) ;
#7828 = ORIENTED_EDGE ( 'NONE', *, *, #24259, .T. ) ;
#7829 = EDGE_LOOP ( 'NONE', ( #725, #6868, #1133, #9342 ) ) ;
#7830 = CARTESIAN_POINT ( 'NONE',  ( 109.7839892703147058, 255.7665025292604071, 41.33169715143176859 ) ) ;
#7831 = ADVANCED_FACE ( 'NONE', ( #9928 ), #8049, .F. ) ;
#7832 = PLANE ( 'NONE',  #11266 ) ;
#7833 = DIRECTION ( 'NONE',  ( -0.000000000000000000, -1.000000000000000000, -0.000000000000000000 ) ) ;
#7834 = DIRECTION ( 'NONE',  ( 0.000000000000000000, 0.000000000000000000, -1.000000000000000000 ) ) ;
#7835 = CARTESIAN_POINT ( 'NONE',  ( 65.00000000000000000, -170.0000000000000853, -75.99999999999997158 ) ) ;
#7836 = CARTESIAN_POINT ( 'NONE',  ( 65.00000000000000000, -150.0000000000000568, -69.99999999999998579 ) ) ;
#7837 = LINE ( 'NONE', #6244, #20479 ) ;
#7838 = CARTESIAN_POINT ( 'NONE',  ( 139.9869122110690114, 197.5248869502487139, -45.00000000000000000 ) ) ;
#7839 = CARTESIAN_POINT ( 'NONE',  ( 187.4999999999996305, 258.6181251126050711, -5.999999999999991118 ) ) ;
#7840 = DIRECTION ( 'NONE',  ( -0.000000000000000000, -0.000000000000000000, 1.000000000000000000 ) ) ;
#7841 = ORIENTED_EDGE ( 'NONE', *, *, #18050, .F. ) ;
#7842 = CARTESIAN_POINT ( 'NONE',  ( -4.528689226187404770, 132.3876760956092085, 15.97891348274549372 ) ) ;
#7843 = VECTOR ( 'NONE', #27880, 1000.000000000000000 ) ;
#7844 = CARTESIAN_POINT ( 'NONE',  ( 107.4212424090118532, 250.1602674884502164, -27.81180689761807301 ) ) ;
#7845 = CARTESIAN_POINT ( 'NONE',  ( 24.13113629555251549, 86.46862463748914251, 99.29534762745656451 ) ) ;
#7846 = CARTESIAN_POINT ( 'NONE',  ( 114.5814157129579058, 230.6339745962151540, -45.00000000000000000 ) ) ;
#7847 = DIRECTION ( 'NONE',  ( 1.000000000000000000, -0.000000000000000000, -0.000000000000000000 ) ) ;
#7848 = ORIENTED_EDGE ( 'NONE', *, *, #8026, .F. ) ;
#7849 = TOROIDAL_SURFACE ( 'NONE', #11542, 72.21503689626331379, 5.000000000000000000 ) ;
#7850 = DIRECTION ( 'NONE',  ( 0.8916010070299166257, -0.4528218681371722343, 0.000000000000000000 ) ) ;
#7851 = VERTEX_POINT ( 'NONE', #22724 ) ;
#7852 = EDGE_CURVE ( 'NONE', #17982, #11545, #17033, .T. ) ;
#7853 = CARTESIAN_POINT ( 'NONE',  ( 158.0000000000015064, 63.00387452705633251, 45.00000000000000000 ) ) ;
#7854 = VERTEX_POINT ( 'NONE', #7634 ) ;
#7855 = EDGE_LOOP ( 'NONE', ( #26394, #805, #6314, #2503 ) ) ;
#7856 = ORIENTED_EDGE ( 'NONE', *, *, #3174, .T. ) ;
#7857 = EDGE_CURVE ( 'NONE', #26178, #18505, #16402, .T. ) ;
#7858 = EDGE_LOOP ( 'NONE', ( #10513, #3648, #19934, #14293 ) ) ;
#7859 = DIRECTION ( 'NONE',  ( 0.000000000000000000, 0.000000000000000000, 1.000000000000000000 ) ) ;
#7860 = CARTESIAN_POINT ( 'NONE',  ( -17.24491960465746132, 80.97823757117562593, 100.0000000000000000 ) ) ;
#7861 = CARTESIAN_POINT ( 'NONE',  ( -212.0372611395816875, -220.0000000000000568, -93.59249812946184477 ) ) ;
#7862 = EDGE_CURVE ( 'NONE', #21781, #18321, #14385, .T. ) ;
#7863 = EDGE_CURVE ( 'NONE', #4812, #13811, #27569, .T. ) ;
#7864 = VECTOR ( 'NONE', #5854, 1000.000000000000114 ) ;
#7865 = EDGE_CURVE ( 'NONE', #23614, #17607, #12009, .T. ) ;
#7866 = CARTESIAN_POINT ( 'NONE',  ( 134.9999999999998579, 455.5353319318992362, -127.0692718809191035 ) ) ;
#7867 = VECTOR ( 'NONE', #3356, 1000.000000000000000 ) ;
#7868 = VECTOR ( 'NONE', #18383, 1000.000000000000000 ) ;
#7869 = CARTESIAN_POINT ( 'NONE',  ( -194.3369914945607491, 63.17511408073718826, 42.65718952139617670 ) ) ;
#7870 = DIRECTION ( 'NONE',  ( 0.000000000000000000, -1.000000000000000000, -1.214306433183764966E-16 ) ) ;
#7871 = CARTESIAN_POINT ( 'NONE',  ( 9.999999999999738876, -50.00000000000004263, 98.28427124746191623 ) ) ;
#7872 = CARTESIAN_POINT ( 'NONE',  ( 129.1910320842563067, 249.4323282239753325, -146.5522648598510216 ) ) ;
#7873 = CARTESIAN_POINT ( 'NONE',  ( -204.3469586999375736, 91.62841992397034119, 29.24611696590164556 ) ) ;
#7874 = SURFACE_STYLE_FILL_AREA ( #9896 ) ;
#7875 = CARTESIAN_POINT ( 'NONE',  ( 157.4999999999998579, 120.9389372034718093, -45.00000000000000000 ) ) ;
#7876 = CARTESIAN_POINT ( 'NONE',  ( 232.4999999999996305, 83.06687458711267880, 36.86484227207694175 ) ) ;
#7877 = EDGE_LOOP ( 'NONE', ( #15489, #19868, #5804, #26646 ) ) ;
#7878 = DIRECTION ( 'NONE',  ( -0.000000000000000000, -0.000000000000000000, -1.000000000000000000 ) ) ;
#7879 = DIRECTION ( 'NONE',  ( 1.000000000000000000, 0.000000000000000000, 0.000000000000000000 ) ) ;
#7881 = ORIENTED_EDGE ( 'NONE', *, *, #4508, .F. ) ;
#7880 = VERTEX_POINT ( 'NONE', #12939 ) ;
#7882 = VECTOR ( 'NONE', #497, 1000.000000000000000 ) ;
#7883 = LINE ( 'NONE', #20958, #16636 ) ;
#7884 = EDGE_LOOP ( 'NONE', ( #20530, #118, #1309, #23904 ) ) ;
#7885 = ORIENTED_EDGE ( 'NONE', *, *, #6941, .T. ) ;
#7886 = VECTOR ( 'NONE', #17280, 1000.000000000000000 ) ;
#7887 =( GEOMETRIC_REPRESENTATION_CONTEXT ( 3 ) GLOBAL_UNCERTAINTY_ASSIGNED_CONTEXT ( ( #15510 ) ) GLOBAL_UNIT_ASSIGNED_CONTEXT ( ( #5050, #13550, #11249 ) ) REPRESENTATION_CONTEXT ( 'NONE', 'WORKASPACE' ) );
#7888 = VERTEX_POINT ( 'NONE', #14953 ) ;
#7889 = VECTOR ( 'NONE', #16170, 1000.000000000000000 ) ;
#7890 = EDGE_CURVE ( 'NONE', #14086, #25161, #23850, .T. ) ;
#7891 = EDGE_LOOP ( 'NONE', ( #15139, #21139, #3458, #20246 ) ) ;
#7892 = ORIENTED_EDGE ( 'NONE', *, *, #5237, .F. ) ;
#7893 = ORIENTED_EDGE ( 'NONE', *, *, #21439, .T. ) ;
#7894 = CARTESIAN_POINT ( 'NONE',  ( 158.0000000000009095, 120.6849996997183183, 45.00000000000000000 ) ) ;
#7895 = EDGE_CURVE ( 'NONE', #21239, #14664, #4304, .T. ) ;
#7896 = LINE ( 'NONE', #3434, #23377 ) ;
#7897 = CARTESIAN_POINT ( 'NONE',  ( 109.9924055441390891, 259.1950347634139575, -44.30286641876279674 ) ) ;
#7898 = FACE_BOUND ( 'NONE', #6124, .T. ) ;
#7899 = AXIS2_PLACEMENT_3D ( 'NONE', #27570, #27712, #7909 ) ;
#7900 = CARTESIAN_POINT ( 'NONE',  ( -272.8608663272381136, -165.2063914494869721, -108.3460931901318673 ) ) ;
#7901 = AXIS2_PLACEMENT_3D ( 'NONE', #3008, #11800, #20539 ) ;
#7902 = FACE_BOUND ( 'NONE', #21379, .T. ) ;
#7903 = CIRCLE ( 'NONE', #18357, 6.000000000000005329 ) ;
#7904 = CARTESIAN_POINT ( 'NONE',  ( -254.3350114625770289, -91.18033988749901653, -16.36034929305424512 ) ) ;
#7905 = VECTOR ( 'NONE', #13955, 999.9999999999998863 ) ;
#7906 = CARTESIAN_POINT ( 'NONE',  ( 110.4484086432434822, 202.7590692334812559, -139.6159404653925549 ) ) ;
#7907 = DIRECTION ( 'NONE',  ( 1.000000000000000000, 0.000000000000000000, 0.000000000000000000 ) ) ;
#7908 = CARTESIAN_POINT ( 'NONE',  ( 232.4999999999996305, 133.0668745871126930, 30.83984227207694317 ) ) ;
#7909 = DIRECTION ( 'NONE',  ( 1.000000000000000000, 3.004539147878382249E-48, -2.775557561562887407E-16 ) ) ;
#7910 = VERTEX_POINT ( 'NONE', #28139 ) ;
#7911 = FACE_OUTER_BOUND ( 'NONE', #21672, .T. ) ;
#7912 = DIRECTION ( 'NONE',  ( 0.4528218681378716193, 0.8916010070295614653, -0.000000000000000000 ) ) ;
#7913 = ORIENTED_EDGE ( 'NONE', *, *, #11624, .F. ) ;
#7914 = APPLICATION_PROTOCOL_DEFINITION ( 'draft international standard', 'automotive_design', 1998, #11879 ) ;
#7915 = ORIENTED_EDGE ( 'NONE', *, *, #4995, .F. ) ;
#7916 = AXIS2_PLACEMENT_3D ( 'NONE', #23515, #14762, #1953 ) ;
#7917 = VERTEX_POINT ( 'NONE', #8479 ) ;
#7918 = EDGE_CURVE ( 'NONE', #10893, #13603, #1865, .T. ) ;
#7919 = AXIS2_PLACEMENT_3D ( 'NONE', #17235, #3, #292 ) ;
#7920 = DIRECTION ( 'NONE',  ( 0.8916010070295719014, -0.4528218681378510246, 0.000000000000000000 ) ) ;
#7921 = DIRECTION ( 'NONE',  ( -1.000000000000000000, 0.000000000000000000, -1.850371707708595943E-15 ) ) ;
#7922 = VERTEX_POINT ( 'NONE', #23563 ) ;
#7923 = VECTOR ( 'NONE', #949, 1000.000000000000000 ) ;
#7924 = ORIENTED_EDGE ( 'NONE', *, *, #1014, .T. ) ;
#7925 = CARTESIAN_POINT ( 'NONE',  ( 158.0000000000008811, 123.1928747072253572, 45.00000000000000000 ) ) ;
#7926 = VECTOR ( 'NONE', #2502, 1000.000000000000000 ) ;
#7927 = CARTESIAN_POINT ( 'NONE',  ( 158.0000000000013642, 76.05112457209858690, 45.00000000000000000 ) ) ;
#7928 = LINE ( 'NONE', #20576, #8679 ) ;
#7929 = ORIENTED_EDGE ( 'NONE', *, *, #25411, .T. ) ;
#7930 = CARTESIAN_POINT ( 'NONE',  ( 232.4999999999996305, 83.06687458711267880, -36.86484227207694175 ) ) ;
#7931 = VERTEX_POINT ( 'NONE', #27852 ) ;
#7932 = LINE ( 'NONE', #3609, #18954 ) ;
#7933 = ADVANCED_FACE ( 'NONE', ( #17234 ), #7849, .T. ) ;
#7934 = EDGE_CURVE ( 'NONE', #14606, #25368, #28278, .T. ) ;
#7935 = LINE ( 'NONE', #18710, #5314 ) ;
#7936 = DIRECTION ( 'NONE',  ( 0.9506505318133544602, 0.3102637045530566295, 0.000000000000000000 ) ) ;
#7937 = CARTESIAN_POINT ( 'NONE',  ( -42.65532241761712839, 131.0044336801082352, -16.34779397420837199 ) ) ;
#7938 = CARTESIAN_POINT ( 'NONE',  ( 139.9999999999999716, -120.0000000000000568, -70.00000000000001421 ) ) ;
#7939 = AXIS2_PLACEMENT_3D ( 'NONE', #3651, #19027, #27635 ) ;
#7940 = DIRECTION ( 'NONE',  ( 1.000000000000000000, 0.000000000000000000, 0.000000000000000000 ) ) ;
#7941 = CARTESIAN_POINT ( 'NONE',  ( -202.4538189947720923, 93.28718049315023109, -30.13672334157483235 ) ) ;
#7942 = ORIENTED_EDGE ( 'NONE', *, *, #25986, .F. ) ;
#7943 = AXIS2_PLACEMENT_3D ( 'NONE', #20464, #3352, #5231 ) ;
#7944 = LINE ( 'NONE', #23174, #27418 ) ;
#7945 = LINE ( 'NONE', #24811, #12440 ) ;
#7946 = CARTESIAN_POINT ( 'NONE',  ( 158.0000000000002558, 181.3818748873943889, 45.00000000000000000 ) ) ;
#7947 = VECTOR ( 'NONE', #11923, 1000.000000000000000 ) ;
#7948 = DIRECTION ( 'NONE',  ( -0.000000000000000000, -0.000000000000000000, 1.000000000000000000 ) ) ;
#7949 = ORIENTED_EDGE ( 'NONE', *, *, #9815, .T. ) ;
#7950 = ADVANCED_FACE ( 'NONE', ( #27995 ), #16818, .T. ) ;
#7951 = DIRECTION ( 'NONE',  ( -0.000000000000000000, -0.000000000000000000, 1.000000000000000000 ) ) ;
#7952 = ORIENTED_EDGE ( 'NONE', *, *, #28236, .T. ) ;
#7953 = EDGE_CURVE ( 'NONE', #21404, #23339, #14662, .T. ) ;
#7954 = CARTESIAN_POINT ( 'NONE',  ( 157.4999999999997158, 263.8878126313725829, 45.00000000000000000 ) ) ;
#7955 = CARTESIAN_POINT ( 'NONE',  ( -143.6428522700808230, 20.24192588826928585, 83.00000000000001421 ) ) ;
#7956 = CARTESIAN_POINT ( 'NONE',  ( 158.0000000000009379, 116.1771246922112653, -45.00000000000000000 ) ) ;
#7957 = ORIENTED_EDGE ( 'NONE', *, *, #24681, .F. ) ;
#7958 = CARTESIAN_POINT ( 'NONE',  ( -310.0000000000001137, -165.0000000000001137, -59.99999999999987210 ) ) ;
#7959 = CARTESIAN_POINT ( 'NONE',  ( 116.5224093497742786, 212.3463313526978595, 45.00000000000000000 ) ) ;
#7960 = ORIENTED_EDGE ( 'NONE', *, *, #1378, .F. ) ;
#7961 = PLANE ( 'NONE',  #4205 ) ;
#7962 = DIRECTION ( 'NONE',  ( -0.000000000000000000, -0.000000000000000000, -1.000000000000000000 ) ) ;
#7963 = EDGE_LOOP ( 'NONE', ( #20925, #2692, #24248, #13344 ) ) ;
#7964 = TOROIDAL_SURFACE ( 'NONE', #14388, 14.95564396479129243, 3.532530335305412716 ) ;
#7965 = ORIENTED_EDGE ( 'NONE', *, *, #21218, .T. ) ;
#7966 = CARTESIAN_POINT ( 'NONE',  ( 158.0000000000008811, 121.1928747072253572, 45.00000000000000000 ) ) ;
#7967 = ORIENTED_EDGE ( 'NONE', *, *, #17860, .T. ) ;
#7968 = VECTOR ( 'NONE', #2608, 1000.000000000000000 ) ;
#7969 = ORIENTED_EDGE ( 'NONE', *, *, #25021, .F. ) ;
#7970 = ORIENTED_EDGE ( 'NONE', *, *, #18816, .F. ) ;
#7971 = AXIS2_PLACEMENT_3D ( 'NONE', #14459, #3521, #5402 ) ;
#7972 = DIRECTION ( 'NONE',  ( -0.8916010070293995948, -0.4528218681381900867, 0.000000000000000000 ) ) ;
#7973 = EDGE_CURVE ( 'NONE', #9462, #13525, #8189, .T. ) ;
#7974 = EDGE_CURVE ( 'NONE', #6716, #4340, #4011, .T. ) ;
#7975 = CARTESIAN_POINT ( 'NONE',  ( 158.0000000000009095, 118.6849996997183041, 45.00000000000000000 ) ) ;
#7976 = CARTESIAN_POINT ( 'NONE',  ( 158.0000000000009663, 113.1613746771971876, 45.00000000000000000 ) ) ;
#7977 = DIRECTION ( 'NONE',  ( -0.8916010070293584056, -0.4528218681382712996, 0.000000000000000000 ) ) ;
#7978 = DIRECTION ( 'NONE',  ( 0.000000000000000000, 0.000000000000000000, -1.000000000000000000 ) ) ;
#7979 = CARTESIAN_POINT ( 'NONE',  ( -224.3698807949888305, 62.17069777283708021, -9.096889663472497389 ) ) ;
#7980 = DIRECTION ( 'NONE',  ( 0.2845658198851049314, -0.9586565047779721516, 0.000000000000000000 ) ) ;
#7981 = FACE_OUTER_BOUND ( 'NONE', #5078, .T. ) ;
#7982 = CARTESIAN_POINT ( 'NONE',  ( 158.0000000000015348, 58.49599951954928656, -45.00000000000000000 ) ) ;
#7983 = DIRECTION ( 'NONE',  ( 0.000000000000000000, 0.000000000000000000, 1.000000000000000000 ) ) ;
#7984 = ORIENTED_EDGE ( 'NONE', *, *, #23138, .F. ) ;
#7985 = CONICAL_SURFACE ( 'NONE', #18990, 6.025000000000002132, 0.7853981633974482790 ) ;
#7986 = EDGE_CURVE ( 'NONE', #223, #4097, #10602, .T. ) ;
#7987 = CARTESIAN_POINT ( 'NONE',  ( 155.4185842870420799, 209.3660254037844481, -45.00000000000000000 ) ) ;
#7988 = CARTESIAN_POINT ( 'NONE',  ( 97.40121527157118919, 241.4156563175464782, -11.01273568327458996 ) ) ;
#7989 = DIRECTION ( 'NONE',  ( 0.4999999999999919509, -0.8660254037844432595, -0.000000000000000000 ) ) ;
#7990 = CYLINDRICAL_SURFACE ( 'NONE', #19655, 5.000000000000004441 ) ;
#7991 = LINE ( 'NONE', #27795, #26685 ) ;
#7992 = CIRCLE ( 'NONE', #27698, 2.000000000000003109 ) ;
#7993 = ORIENTED_EDGE ( 'NONE', *, *, #6467, .T. ) ;
#7994 = EDGE_CURVE ( 'NONE', #13277, #27664, #21545, .T. ) ;
#7995 = EDGE_CURVE ( 'NONE', #9638, #17008, #6312, .T. ) ;
#7996 = CARTESIAN_POINT ( 'NONE',  ( 217.4999999999996305, 194.4107529906318064, 75.35061095560300259 ) ) ;
#7997 = ORIENTED_EDGE ( 'NONE', *, *, #8866, .F. ) ;
#7998 = DIRECTION ( 'NONE',  ( 0.8916010070293383105, -0.4528218681383106015, 0.000000000000000000 ) ) ;
#7999 = ORIENTED_EDGE ( 'NONE', *, *, #16495, .T. ) ;
#8000 = EDGE_CURVE ( 'NONE', #18031, #17928, #23417, .T. ) ;
#8001 = ORIENTED_EDGE ( 'NONE', *, *, #9034, .F. ) ;
#8002 = CARTESIAN_POINT ( 'NONE',  ( -85.27280602623865491, 136.4561170694882435, 13.48388367063513371 ) ) ;
#8003 = APPLICATION_CONTEXT ( 'automotive_design' ) ;
#8004 = VERTEX_POINT ( 'NONE', #3726 ) ;
#8005 = ORIENTED_EDGE ( 'NONE', *, *, #26997, .T. ) ;
#8006 = CARTESIAN_POINT ( 'NONE',  ( -260.0000000000001137, -220.0000000000000853, 60.00000000000002132 ) ) ;
#8007 = VECTOR ( 'NONE', #9818, 1000.000000000000000 ) ;
#8008 = CARTESIAN_POINT ( 'NONE',  ( 157.4999999999998579, 53.22631200078164682, -45.00000000000000000 ) ) ;
#8009 = FACE_OUTER_BOUND ( 'NONE', #21384, .T. ) ;
#8010 = FACE_OUTER_BOUND ( 'NONE', #21443, .T. ) ;
#8011 = VECTOR ( 'NONE', #14923, 1000.000000000000000 ) ;
#8012 = CARTESIAN_POINT ( 'NONE',  ( -13.93137870332982331, 8.043285244550061108, -45.00000000000000000 ) ) ;
#8013 = CARTESIAN_POINT ( 'NONE',  ( -272.5977457686555567, -170.1167710987052146, 87.25339983416321843 ) ) ;
#8014 = CARTESIAN_POINT ( 'NONE',  ( 134.6025894306528699, 250.0000000000000568, -151.0000000000000284 ) ) ;
#8015 = CARTESIAN_POINT ( 'NONE',  ( -222.7951581118867068, 86.58804311865961267, 17.41104556328208375 ) ) ;
#8016 = CARTESIAN_POINT ( 'NONE',  ( -41.04971513216914047, 194.3765543069588659, 45.00000000000000000 ) ) ;
#8017 = CARTESIAN_POINT ( 'NONE',  ( 157.9999999999996589, 274.1732501651540588, 45.00000000000000000 ) ) ;
#8018 = FACE_OUTER_BOUND ( 'NONE', #27729, .T. ) ;
#8019 = VERTEX_POINT ( 'NONE', #2 ) ;
#8020 = CARTESIAN_POINT ( 'NONE',  ( 179.9999999999999147, 494.4107529906318632, -100.0000000000000142 ) ) ;
#8021 = CARTESIAN_POINT ( 'NONE',  ( 106.6443156122982572, 210.2031273749746276, -143.0663072493379104 ) ) ;
#8022 = EDGE_CURVE ( 'NONE', #11217, #7779, #8335, .T. ) ;
#8024 = ORIENTED_EDGE ( 'NONE', *, *, #14271, .T. ) ;
#8023 = ORIENTED_EDGE ( 'NONE', *, *, #8866, .T. ) ;
#8025 = CIRCLE ( 'NONE', #20855, 5.000000000000004441 ) ;
#8026 = EDGE_CURVE ( 'NONE', #8626, #7922, #10633, .T. ) ;
#8027 = DIRECTION ( 'NONE',  ( -0.000000000000000000, 0.000000000000000000, -1.000000000000000000 ) ) ;
#8028 = EDGE_CURVE ( 'NONE', #11012, #22407, #18855, .T. ) ;
#8029 = ORIENTED_EDGE ( 'NONE', *, *, #24293, .T. ) ;
#8030 = VERTEX_POINT ( 'NONE', #9339 ) ;
#8031 = CIRCLE ( 'NONE', #27738, 67.21503689626328537 ) ;
#8032 = ORIENTED_EDGE ( 'NONE', *, *, #15983, .F. ) ;
#8033 = ORIENTED_EDGE ( 'NONE', *, *, #15633, .T. ) ;
#8034 = ORIENTED_EDGE ( 'NONE', *, *, #24237, .T. ) ;
#8035 = VERTEX_POINT ( 'NONE', #574 ) ;
#8036 = CARTESIAN_POINT ( 'NONE',  ( 367.4999999999996021, 44.41075299063183479, 100.0000000000000284 ) ) ;
#8037 = DIRECTION ( 'NONE',  ( 1.000000000000000000, 4.163336342344337027E-16, 0.000000000000000000 ) ) ;
#8038 = VECTOR ( 'NONE', #20622, 1000.000000000000000 ) ;
#8039 = AXIS2_PLACEMENT_3D ( 'NONE', #22361, #2668, #17472 ) ;
#8040 = AXIS2_PLACEMENT_3D ( 'NONE', #8587, #13052, #13466 ) ;
#8041 = CARTESIAN_POINT ( 'NONE',  ( 109.9999999999999005, 260.0000000000000000, -45.00000000000000000 ) ) ;
#8042 = CARTESIAN_POINT ( 'NONE',  ( -23.68004821426667661, 128.1049817043144117, -17.45875844069260907 ) ) ;
#8043 = CARTESIAN_POINT ( 'NONE',  ( 79.99999999999991473, 140.0000000000000000, 45.00000000000000000 ) ) ;
#8044 = CIRCLE ( 'NONE', #4842, 11.42311362948588105 ) ;
#8045 = DIRECTION ( 'NONE',  ( 0.000000000000000000, -0.000000000000000000, -1.000000000000000000 ) ) ;
#8046 = CARTESIAN_POINT ( 'NONE',  ( -207.6005680426152082, 75.52797596137341429, -42.89671038906845979 ) ) ;
#8047 = CARTESIAN_POINT ( 'NONE',  ( 112.0145559484521414, 200.7200133411070908, -141.9885977063034943 ) ) ;
#8048 = FACE_OUTER_BOUND ( 'NONE', #8316, .T. ) ;
#8049 = PLANE ( 'NONE',  #11072 ) ;
#8050 = CARTESIAN_POINT ( 'NONE',  ( 167.4999999999996589, 526.4263741777961059, -74.99999999999995737 ) ) ;
#8051 = ORIENTED_EDGE ( 'NONE', *, *, #13749, .T. ) ;
#8052 = DIRECTION ( 'NONE',  ( 1.000000000000000000, 0.000000000000000000, 0.000000000000000000 ) ) ;
#8053 = EDGE_CURVE ( 'NONE', #23149, #23826, #5012, .T. ) ;
#8054 = EDGE_CURVE ( 'NONE', #20648, #7226, #24836, .T. ) ;
#8055 = FACE_OUTER_BOUND ( 'NONE', #7397, .T. ) ;
#8056 = VERTEX_POINT ( 'NONE', #141 ) ;
#8058 = B_SPLINE_CURVE_WITH_KNOTS ( 'NONE', 3,
 ( #7698, #16461, #15909, #4960, #13751, #2808, #25496, #12302, #10275 ),
 .UNSPECIFIED., .F., .F.,
 ( 4, 2, 1, 2, 4 ),
 ( 0.000000000000000000, 0.003850132855190869542, 0.007700265710381739084, 0.01155039856557260949, 0.01540053142076347817 ),
 .UNSPECIFIED. ) ;
#8057 = DIRECTION ( 'NONE',  ( 0.000000000000000000, 0.9242245927363030855, 0.3818493186865927203 ) ) ;
#8059 = AXIS2_PLACEMENT_3D ( 'NONE', #2194, #2336, #26053 ) ;
#8060 = ORIENTED_EDGE ( 'NONE', *, *, #41, .T. ) ;
#8061 = VECTOR ( 'NONE', #24479, 1000.000000000000000 ) ;
#8062 = VECTOR ( 'NONE', #5202, 1000.000000000000000 ) ;
#8063 = VERTEX_POINT ( 'NONE', #7034 ) ;
#8064 = CARTESIAN_POINT ( 'NONE',  ( 157.9999999999996589, 278.6811251726610976, -45.00000000000000000 ) ) ;
#8065 = DIRECTION ( 'NONE',  ( -4.540956701092242152E-16, -1.000000000000000000, -0.000000000000000000 ) ) ;
#8066 = VERTEX_POINT ( 'NONE', #26415 ) ;
#8067 = VECTOR ( 'NONE', #19917, 1000.000000000000000 ) ;
#8068 = ORIENTED_EDGE ( 'NONE', *, *, #1946, .F. ) ;
#8069 = CARTESIAN_POINT ( 'NONE',  ( 158.0000000000000568, 201.4448749474510407, 45.00000000000000000 ) ) ;
#8070 = CARTESIAN_POINT ( 'NONE',  ( 158.0000000000002274, 185.8897498949014278, 45.00000000000000000 ) ) ;
#8071 = FACE_OUTER_BOUND ( 'NONE', #19006, .T. ) ;
#8072 = ORIENTED_EDGE ( 'NONE', *, *, #27412, .T. ) ;
#8073 = CARTESIAN_POINT ( 'NONE',  ( 104.4199312700443016, 89.58810137558876363, 100.0000000000000142 ) ) ;
#8074 = ORIENTED_EDGE ( 'NONE', *, *, #13050, .F. ) ;
#8075 = DIRECTION ( 'NONE',  ( -0.000000000000000000, -0.000000000000000000, 1.000000000000000000 ) ) ;
#8076 = DIRECTION ( 'NONE',  ( 0.000000000000000000, 0.000000000000000000, -1.000000000000000000 ) ) ;
#8077 = EDGE_CURVE ( 'NONE', #1913, #15391, #24413, .T. ) ;
#8078 = CARTESIAN_POINT ( 'NONE',  ( -40.35434868956970433, 130.4209029819868704, -15.14570054738094562 ) ) ;
#8079 = DIRECTION ( 'NONE',  ( 4.163336342344337027E-16, -1.000000000000000000, 1.387778780781445429E-16 ) ) ;
#8080 = AXIS2_PLACEMENT_3D ( 'NONE', #12954, #6618, #19552 ) ;
#8081 = CARTESIAN_POINT ( 'NONE',  ( 217.4999999999996305, 83.06687458711267880, -30.86484227207694886 ) ) ;
#8082 = CARTESIAN_POINT ( 'NONE',  ( -191.3943905361025770, 102.1783726111194852, -32.85579694620437863 ) ) ;
#8083 = EDGE_CURVE ( 'NONE', #2726, #23391, #15665, .T. ) ;
#8084 = EDGE_LOOP ( 'NONE', ( #2332, #11399 ) ) ;
#8085 = DIRECTION ( 'NONE',  ( -0.8916010070299064116, 0.4528218681371922183, 0.000000000000000000 ) ) ;
#8086 =( BOUNDED_SURFACE ( )  B_SPLINE_SURFACE ( 3, 2, ( 
 ( #25773, #4223, #14733 ),
 ( #14882, #19458, #21328 ),
 ( #21609, #23486, #4080 ),
 ( #3803, #21466, #6101 ),
 ( #12867, #21760, #23631 ),
 ( #1647, #15163, #10559 ),
 ( #1780, #1510, #28059 ),
 ( #27784, #12589, #8405 ),
 ( #25918, #23914, #17160 ),
 ( #2066, #6242, #19035 ),
 ( #26058, #8264, #3941 ),
 ( #13014, #15017, #10704 ),
 ( #14591, #25634, #10417 ),
 ( #10842, #12727, #23347 ),
 ( #19600, #23768, #7979 ),
 ( #6381, #1921, #28202 ),
 ( #8121, #19171, #16747 ),
 ( #8549, #17297, #16881 ),
 ( #25501, #5817, #3658 ),
 ( #12446, #21185, #27916 ),
 ( #17017, #5327, #27158 ),
 ( #3160, #22287, #459 ),
 ( #7495, #22854, #24442 ),
 ( #11950, #319, #5186 ),
 ( #11533, #20126, #20552 ),
 ( #9368, #20273, #2598 ),
 ( #13973, #20414, #16260 ),
 ( #605, #22579, #22721 ),
 ( #9073, #4752, #26735 ),
 ( #13828, #13537, #3024 ),
 ( #18126, #11812, #14104 ),
 ( #17831, #2741, #9218 ),
 ( #26884, #7208, #877 ),
 ( #24586, #9648, #6912 ),
 ( #18405, #2889, #11382 ),
 ( #22431, #15981, #15692 ),
 ( #17980, #25012, #26584 ),
 ( #13684, #7059, #15843 ),
 ( #24732, #4894, #11678 ),
 ( #5040, #742, #9511 ),
 ( #18266, #27017, #7353 ),
 ( #16121, #24872, #25705 ),
 ( #16951, #27426, #1294 ),
 ( #3722, #5608, #16399 ),
 ( #7769, #16812, #20973 ),
 ( #5746, #18819, #23278 ) ),
 .UNSPECIFIED., .F., .F., .F. ) 
 B_SPLINE_SURFACE_WITH_KNOTS ( ( 4, 2, 2, 2, 2, 2, 2, 2, 2, 2, 2, 2, 2, 2, 2, 2, 2, 2, 2, 2, 2, 2, 4 ),
 ( 3, 3 ),
 ( -1.040834085586084257E-17, 0.004062158184156347031, 0.008124316368312704470, 0.01015539546039088276, 0.01218647455246906278, 0.01624863273662541935, 0.01827971182870359590, 0.02031079092078177592, 0.02437294910493813249, 0.02640402819701630904, 0.02843510728909448906, 0.03249726547325084564, 0.03655942365740720568, 0.03859050274948538223, 0.04062158184156355878, 0.04468374002571991882, 0.04874589820987627886, 0.05280805639403263196, 0.05687021457818899201, 0.05890129367026716856, 0.06093237276234535205, 0.06296345185442353554, 0.06499453094650170515 ),
 ( 0.000000000000000000, 1.000000000000000000 ),
 .UNSPECIFIED. ) 
 GEOMETRIC_REPRESENTATION_ITEM ( )  RATIONAL_B_SPLINE_SURFACE ( (
 ( 1.000000000000000000, 0.7071067811865475727, 1.000000000000000000),
 ( 1.000000000000000000, 0.7127618277282021797, 1.000000000000000000),
 ( 1.000000000000000000, 0.7177019917273029792, 1.000000000000000000),
 ( 1.000000000000000000, 0.7259809929037955856, 1.000000000000000000),
 ( 1.000000000000000000, 0.7293222386929405499, 1.000000000000000000),
 ( 1.000000000000000000, 0.7329411530155929277, 1.000000000000000000),
 ( 1.000000000000000000, 0.7339161091547367066, 1.000000000000000000),
 ( 1.000000000000000000, 0.7353380047207777048, 1.000000000000000000),
 ( 1.000000000000000000, 0.7357895841719410690, 1.000000000000000000),
 ( 1.000000000000000000, 0.7363489957920964502, 1.000000000000000000),
 ( 1.000000000000000000, 0.7356640979630035826, 1.000000000000000000),
 ( 1.000000000000000000, 0.7329334158298154156, 1.000000000000000000),
 ( 1.000000000000000000, 0.7317386460501513756, 1.000000000000000000),
 ( 1.000000000000000000, 0.7287527534628306380, 1.000000000000000000),
 ( 1.000000000000000000, 0.7269678409233529814, 1.000000000000000000),
 ( 1.000000000000000000, 0.7207930214947959602, 1.000000000000000000),
 ( 1.000000000000000000, 0.7155672824331829052, 1.000000000000000000),
 ( 1.000000000000000000, 0.7060917826293188204, 1.000000000000000000),
 ( 1.000000000000000000, 0.7026601427809967548, 1.000000000000000000),
 ( 1.000000000000000000, 0.6952527892509502427, 1.000000000000000000),
 ( 1.000000000000000000, 0.6912624871067051258, 1.000000000000000000),
 ( 1.000000000000000000, 0.6786163957653905676, 1.000000000000000000),
 ( 1.000000000000000000, 0.6692836425643465814, 1.000000000000000000),
 ( 1.000000000000000000, 0.6490371914779309304, 1.000000000000000000),
 ( 1.000000000000000000, 0.6381215166341221989, 1.000000000000000000),
 ( 1.000000000000000000, 0.6207537710089482408, 1.000000000000000000),
 ( 1.000000000000000000, 0.6147992736454299667, 1.000000000000000000),
 ( 1.000000000000000000, 0.6026007117946927671, 1.000000000000000000),
 ( 1.000000000000000000, 0.5963421480512035577, 1.000000000000000000),
 ( 1.000000000000000000, 0.5773189341497990679, 1.000000000000000000),
 ( 1.000000000000000000, 0.5643376819679217782, 1.000000000000000000),
 ( 1.000000000000000000, 0.5383412250590065007, 1.000000000000000000),
 ( 1.000000000000000000, 0.5253226519624610846, 1.000000000000000000),
 ( 1.000000000000000000, 0.5000277150692035155, 1.000000000000000000),
 ( 1.000000000000000000, 0.4877436159665405335, 1.000000000000000000),
 ( 1.000000000000000000, 0.4650351994093656072, 1.000000000000000000),
 ( 1.000000000000000000, 0.4547962088601842923, 1.000000000000000000),
 ( 1.000000000000000000, 0.4420154047700521338, 1.000000000000000000),
 ( 1.000000000000000000, 0.4381857281609657373, 1.000000000000000000),
 ( 1.000000000000000000, 0.4315381087321277787, 1.000000000000000000),
 ( 1.000000000000000000, 0.4287205967313478805, 1.000000000000000000),
 ( 1.000000000000000000, 0.4242344318730199015, 1.000000000000000000),
 ( 1.000000000000000000, 0.4225662398543922893, 1.000000000000000000),
 ( 1.000000000000000000, 0.4204880647989017173, 1.000000000000000000),
 ( 1.000000000000000000, 0.4200800889062838439, 1.000000000000000000),
 ( 1.000000000000000000, 0.4203293914240995299, 1.000000000000000000) ) ) 
 REPRESENTATION_ITEM ( '' )  SURFACE ( )  );
#8088 = CARTESIAN_POINT ( 'NONE',  ( 158.0000000000015632, 55.98812451204224061, 45.00000000000000000 ) ) ;
#8087 = AXIS2_PLACEMENT_3D ( 'NONE', #18616, #25220, #23073 ) ;
#8089 = CARTESIAN_POINT ( 'NONE',  ( 157.9999999999998010, 241.0630000600560550, 45.00000000000000000 ) ) ;
#8090 = LINE ( 'NONE', #21435, #26330 ) ;
#8091 = ORIENTED_EDGE ( 'NONE', *, *, #22289, .F. ) ;
#8092 = DIRECTION ( 'NONE',  ( 0.000000000000000000, 0.000000000000000000, -1.000000000000000000 ) ) ;
#8093 = ORIENTED_EDGE ( 'NONE', *, *, #12791, .T. ) ;
#8094 = ADVANCED_FACE ( 'NONE', ( #13226 ), #18100, .F. ) ;
#8095 = CARTESIAN_POINT ( 'NONE',  ( 0.000000000000000000, -18.01420295945611727, 100.0000000000000000 ) ) ;
#8096 = LINE ( 'NONE', #20738, #1833 ) ;
#8097 = CARTESIAN_POINT ( 'NONE',  ( -305.0000000000001137, -165.0000000000001137, 60.00000000000002842 ) ) ;
#8098 = ORIENTED_EDGE ( 'NONE', *, *, #14481, .T. ) ;
#8099 = DIRECTION ( 'NONE',  ( 1.000000000000000000, 0.000000000000000000, 0.000000000000000000 ) ) ;
#8100 = CARTESIAN_POINT ( 'NONE',  ( 157.9999999999996589, 276.1732501651540588, 45.00000000000000000 ) ) ;
#8101 = ORIENTED_EDGE ( 'NONE', *, *, #26992, .T. ) ;
#8102 = EDGE_CURVE ( 'NONE', #20337, #11428, #6886, .T. ) ;
#8103 = CARTESIAN_POINT ( 'NONE',  ( 158.0000000000005400, 153.7952498048169048, 45.00000000000000000 ) ) ;
#8104 = CARTESIAN_POINT ( 'NONE',  ( 232.4999999999996305, 133.0668745871126930, 36.86484227207694886 ) ) ;
#8105 = ORIENTED_EDGE ( 'NONE', *, *, #3994, .T. ) ;
#8106 = AXIS2_PLACEMENT_3D ( 'NONE', #11260, #19723, #4481 ) ;
#8107 = ORIENTED_EDGE ( 'NONE', *, *, #11215, .T. ) ;
#8108 = DIRECTION ( 'NONE',  ( -0.000000000000000000, -0.000000000000000000, -1.000000000000000000 ) ) ;
#8109 = VERTEX_POINT ( 'NONE', #21970 ) ;
#8110 = AXIS2_PLACEMENT_3D ( 'NONE', #18164, #26918, #7243 ) ;
#8111 = ORIENTED_EDGE ( 'NONE', *, *, #26805, .F. ) ;
#8112 = ORIENTED_EDGE ( 'NONE', *, *, #3562, .F. ) ;
#8113 = EDGE_CURVE ( 'NONE', #14425, #26178, #13803, .T. ) ;
#8114 = LINE ( 'NONE', #23759, #3336 ) ;
#8115 = LINE ( 'NONE', #3653, #5277 ) ;
#8116 = DIRECTION ( 'NONE',  ( 0.000000000000000000, 1.000000000000000000, 0.000000000000000000 ) ) ;
#8117 = CARTESIAN_POINT ( 'NONE',  ( -71.37541315349507443, 230.0000000000000000, 15.00000000000000000 ) ) ;
#8118 = CARTESIAN_POINT ( 'NONE',  ( -200.0000000000000284, -62.36067977499792647, 25.00000000000000000 ) ) ;
#8119 = LINE ( 'NONE', #16880, #23651 ) ;
#8120 = EDGE_CURVE ( 'NONE', #4661, #21276, #9706, .T. ) ;
#8121 = CARTESIAN_POINT ( 'NONE',  ( -223.4403667166176604, 71.79593500864021394, -19.27754551403313599 ) ) ;
#8122 = DIRECTION ( 'NONE',  ( -0.8790438869537371414, -0.4767408570798871148, -0.000000000000000000 ) ) ;
#8123 = CARTESIAN_POINT ( 'NONE',  ( 0.03761738457578049644, -1.249999999999998668, -7.196727321902812946 ) ) ;
#8124 = CARTESIAN_POINT ( 'NONE',  ( 157.4999999999998010, 238.8090625563025071, -45.00000000000000000 ) ) ;
#8125 = VECTOR ( 'NONE', #20711, 1000.000000000000000 ) ;
#8126 = ORIENTED_EDGE ( 'NONE', *, *, #25021, .T. ) ;
#8127 = FACE_OUTER_BOUND ( 'NONE', #1765, .T. ) ;
#8128 = VECTOR ( 'NONE', #11911, 1000.000000000000000 ) ;
#8129 = CARTESIAN_POINT ( 'NONE',  ( 134.9999999999998579, 220.0000000000000284, -100.0000000000000142 ) ) ;
#8130 = CARTESIAN_POINT ( 'NONE',  ( 14.18877312265928659, 89.71084980560162592, 98.38498031279395661 ) ) ;
#8131 = LINE ( 'NONE', #16480, #19243 ) ;
#8132 = LINE ( 'NONE', #25646, #5593 ) ;
#8133 = ORIENTED_EDGE ( 'NONE', *, *, #12522, .T. ) ;
#8134 = EDGE_CURVE ( 'NONE', #11070, #11107, #26702, .T. ) ;
#8135 = CARTESIAN_POINT ( 'NONE',  ( 157.4999999999998579, 135.9861872485140850, 45.00000000000000000 ) ) ;
#8136 = ORIENTED_EDGE ( 'NONE', *, *, #3391, .T. ) ;
#8137 = PLANE ( 'NONE',  #19976 ) ;
#8138 = VERTEX_POINT ( 'NONE', #22549 ) ;
#8139 = ORIENTED_EDGE ( 'NONE', *, *, #14492, .T. ) ;
#8140 = CARTESIAN_POINT ( 'NONE',  ( -92.83229342711496201, 134.7610587320406239, 15.46096080868298550 ) ) ;
#8141 = ORIENTED_EDGE ( 'NONE', *, *, #3636, .F. ) ;
#8142 = ORIENTED_EDGE ( 'NONE', *, *, #4671, .T. ) ;
#8143 = CARTESIAN_POINT ( 'NONE',  ( 112.6399768800337284, 222.5565040444928115, 96.77053691278567271 ) ) ;
#8144 = AXIS2_PLACEMENT_3D ( 'NONE', #13074, #15079, #26120 ) ;
#8145 = EDGE_CURVE ( 'NONE', #25647, #8109, #11354, .T. ) ;
#8146 = FACE_OUTER_BOUND ( 'NONE', #16646, .T. ) ;
#8147 = CARTESIAN_POINT ( 'NONE',  ( -210.8169819562698137, -219.6631312228495574, 91.44098042302121598 ) ) ;
#8148 = CARTESIAN_POINT ( 'NONE',  ( -144.0689309099013258, 125.7628306214139116, -18.57776427790886231 ) ) ;
#8149 = EDGE_CURVE ( 'NONE', #15078, #10864, #8907, .T. ) ;
#8150 = LINE ( 'NONE', #8294, #7362 ) ;
#8151 = LINE ( 'NONE', #27672, #23338 ) ;
#8152 = CARTESIAN_POINT ( 'NONE',  ( 30.92500016277389108, -41.52323098288959358, 99.96966619038498436 ) ) ;
#8153 = CARTESIAN_POINT ( 'NONE',  ( -230.8220000157087668, 92.55346088012031203, -13.02757477273544851 ) ) ;
#8154 = CARTESIAN_POINT ( 'NONE',  ( 129.7913655954319836, 249.5452024337660646, -148.0040471605077812 ) ) ;
#8155 = CARTESIAN_POINT ( 'NONE',  ( -207.1201485044495030, 89.67250137467401316, 27.42661007367943071 ) ) ;
#8156 = EDGE_CURVE ( 'NONE', #14497, #9601, #4580, .T. ) ;
#8157 = PLANE ( 'NONE',  #6932 ) ;
#8158 = DIRECTION ( 'NONE',  ( -0.8916010070293383105, -0.4528218681383106015, 0.000000000000000000 ) ) ;
#8159 = LINE ( 'NONE', #3695, #12070 ) ;
#8160 = VERTEX_POINT ( 'NONE', #20389 ) ;
#8161 = AXIS2_PLACEMENT_3D ( 'NONE', #11498, #2852, #850 ) ;
#8162 = CARTESIAN_POINT ( 'NONE',  ( 157.9999999999996589, 271.6653751576470768, 45.00000000000000000 ) ) ;
#8163 = CARTESIAN_POINT ( 'NONE',  ( 185.9255560592262100, 121.0883471088020116, 45.00000000000000000 ) ) ;
#8164 = PLANE ( 'NONE',  #22562 ) ;
#8166 = VERTEX_POINT ( 'NONE', #432 ) ;
#8165 = ORIENTED_EDGE ( 'NONE', *, *, #25672, .T. ) ;
#8167 = CARTESIAN_POINT ( 'NONE',  ( 105.7413873646182765, 247.3652972445293017, -29.41146778674738371 ) ) ;
#8168 = EDGE_LOOP ( 'NONE', ( #641, #10959, #18737, #23162 ) ) ;
#8169 = ORIENTED_EDGE ( 'NONE', *, *, #8054, .T. ) ;
#8170 = EDGE_LOOP ( 'NONE', ( #20139, #1826, #7795, #11521, #2046, #8165, #5445, #834, #17214, #14649 ) ) ;
#8171 = AXIS2_PLACEMENT_3D ( 'NONE', #22672, #15930, #18496 ) ;
#8172 = ORIENTED_EDGE ( 'NONE', *, *, #17061, .T. ) ;
#8173 = VERTEX_POINT ( 'NONE', #9194 ) ;
#8174 = ORIENTED_EDGE ( 'NONE', *, *, #11047, .T. ) ;
#8175 = CARTESIAN_POINT ( 'NONE',  ( 134.9999999999998579, 220.0000000000000284, -45.00000000000000000 ) ) ;
#8176 = VECTOR ( 'NONE', #9723, 1000.000000000000000 ) ;
#8177 = CIRCLE ( 'NONE', #7270, 30.00000000000001421 ) ;
#8178 = FACE_BOUND ( 'NONE', #1422, .T. ) ;
#8179 = EDGE_CURVE ( 'NONE', #6129, #4617, #8761, .T. ) ;
#8180 = DIRECTION ( 'NONE',  ( -0.000000000000000000, -0.000000000000000000, -1.000000000000000000 ) ) ;
#8181 = EDGE_CURVE ( 'NONE', #21558, #4484, #11504, .T. ) ;
#8182 = CARTESIAN_POINT ( 'NONE',  ( 9.345921402568846403, 139.9999999999999716, -15.00000000000000000 ) ) ;
#8183 = CYLINDRICAL_SURFACE ( 'NONE', #10774, 5.999999999999991118 ) ;
#8184 = CARTESIAN_POINT ( 'NONE',  ( 158.0000000000006537, 143.7637497747887210, 45.00000000000000000 ) ) ;
#8185 = CARTESIAN_POINT ( 'NONE',  ( -210.7172313291012529, 103.7585653882801182, 5.000000000000002665 ) ) ;
#8187 = AXIS2_PLACEMENT_3D ( 'NONE', #5610, #20975, #14523 ) ;
#8186 = CARTESIAN_POINT ( 'NONE',  ( 110.6502358794795100, 202.4751799119059115, -139.8013169873308641 ) ) ;
#8188 = PLANE ( 'NONE',  #1324 ) ;
#8189 = LINE ( 'NONE', #2002, #15654 ) ;
#8190 = CARTESIAN_POINT ( 'NONE',  ( 158.0000000000002558, 183.3818748873943889, 45.00000000000000000 ) ) ;
#8191 = ORIENTED_EDGE ( 'NONE', *, *, #13766, .F. ) ;
#8192 = CARTESIAN_POINT ( 'NONE',  ( -196.7966726397505681, 98.32233333166497857, 31.72664882486916937 ) ) ;
#8193 = CIRCLE ( 'NONE', #25642, 30.00000000000000000 ) ;
#8194 = PRODUCT_DEFINITION_SHAPE ( 'NONE', 'NONE',  #13176 ) ;
#8195 = EDGE_CURVE ( 'NONE', #22168, #26863, #9772, .T. ) ;
#8196 = VECTOR ( 'NONE', #11564, 1000.000000000000000 ) ;
#8197 = DIRECTION ( 'NONE',  ( 1.000000000000000000, 3.469446951953614189E-16, -0.000000000000000000 ) ) ;
#8198 = ORIENTED_EDGE ( 'NONE', *, *, #11660, .F. ) ;
#8199 = SHAPE_DEFINITION_REPRESENTATION ( #14625, #18912 ) ;
#8200 = ORIENTED_EDGE ( 'NONE', *, *, #13975, .F. ) ;
#8202 = ORIENTED_EDGE ( 'NONE', *, *, #20931, .F. ) ;
#8201 = VECTOR ( 'NONE', #7792, 1000.000000000000000 ) ;
#8203 = CARTESIAN_POINT ( 'NONE',  ( 111.0641325991587252, 99.15168937823351314, 100.0000000000000142 ) ) ;
#8204 = EDGE_CURVE ( 'NONE', #6807, #9810, #1853, .T. ) ;
#8205 = CARTESIAN_POINT ( 'NONE',  ( 158.0000000000011369, 96.11412463215494029, 45.00000000000000000 ) ) ;
#8206 = ORIENTED_EDGE ( 'NONE', *, *, #27503, .F. ) ;
#8207 = ORIENTED_EDGE ( 'NONE', *, *, #1721, .T. ) ;
#8208 = CARTESIAN_POINT ( 'NONE',  ( 158.0000000000001137, 195.9212499249295831, 45.00000000000000000 ) ) ;
#8209 = CYLINDRICAL_SURFACE ( 'NONE', #10220, 5.999999999999991118 ) ;
#8210 = AXIS2_PLACEMENT_3D ( 'NONE', #24452, #11096, #8939 ) ;
#8211 = CARTESIAN_POINT ( 'NONE',  ( -187.3345487617074809, 105.2479335822991970, -31.76775584780962802 ) ) ;
#8212 = ORIENTED_EDGE ( 'NONE', *, *, #9091, .T. ) ;
#8213 = EDGE_CURVE ( 'NONE', #14958, #1247, #9622, .T. ) ;
#8214 = CARTESIAN_POINT ( 'NONE',  ( 118.4313905926795769, 122.3304618272157285, 100.0000000000000142 ) ) ;
#8215 = ORIENTED_EDGE ( 'NONE', *, *, #22893, .T. ) ;
#8216 = LINE ( 'NONE', #3899, #10719 ) ;
#8217 = EDGE_CURVE ( 'NONE', #19122, #18428, #12349, .T. ) ;
#8218 = AXIS2_PLACEMENT_3D ( 'NONE', #21232, #27541, #3272 ) ;
#8219 = EDGE_CURVE ( 'NONE', #2800, #10, #14357, .T. ) ;
#8220 = DIRECTION ( 'NONE',  ( -1.000000000000000000, 0.000000000000000000, 0.000000000000000000 ) ) ;
#8221 = FACE_OUTER_BOUND ( 'NONE', #17140, .T. ) ;
#8222 = AXIS2_PLACEMENT_3D ( 'NONE', #19599, #28339, #2341 ) ;
#8223 = AXIS2_PLACEMENT_3D ( 'NONE', #22103, #17647, #272 ) ;
#8224 = DIRECTION ( 'NONE',  ( 0.8916010070293584056, -0.4528218681382712996, 0.000000000000000000 ) ) ;
#8225 = CARTESIAN_POINT ( 'NONE',  ( 158.0000000000000000, 206.4606249624626457, 45.00000000000000000 ) ) ;
#8226 = ORIENTED_EDGE ( 'NONE', *, *, #10910, .T. ) ;
#8227 = LINE ( 'NONE', #15271, #19645 ) ;
#8228 = DIRECTION ( 'NONE',  ( -1.000000000000000000, 0.000000000000000000, 0.000000000000000000 ) ) ;
#8229 = DIRECTION ( 'NONE',  ( 0.4528218681375913990, 0.8916010070297037959, -0.000000000000000000 ) ) ;
#8230 = LINE ( 'NONE', #8371, #196 ) ;
#8231 = ORIENTED_EDGE ( 'NONE', *, *, #19170, .T. ) ;
#8232 = CARTESIAN_POINT ( 'NONE',  ( -277.2150368962633706, -237.2150368962634559, 90.00000000000002842 ) ) ;
#8233 = AXIS2_PLACEMENT_3D ( 'NONE', #18135, #5192, #11685 ) ;
#8234 = DIRECTION ( 'NONE',  ( -0.8916010070299774659, 0.4528218681370523302, 0.000000000000000000 ) ) ;
#8235 = CARTESIAN_POINT ( 'NONE',  ( 79.99999999999994316, -40.00000000000002842, 100.0000000000000142 ) ) ;
#8236 = CARTESIAN_POINT ( 'NONE',  ( -217.8036320994844175, 87.77465520521086262, 17.64589920944733592 ) ) ;
#8237 = EDGE_LOOP ( 'NONE', ( #12851, #26995, #14752, #17668 ) ) ;
#8238 = CIRCLE ( 'NONE', #15584, 7.507013428474183847 ) ;
#8239 = DIRECTION ( 'NONE',  ( -0.000000000000000000, -0.000000000000000000, -1.000000000000000000 ) ) ;
#8240 = VERTEX_POINT ( 'NONE', #5159 ) ;
#8241 = VECTOR ( 'NONE', #10714, 1000.000000000000000 ) ;
#8242 = LINE ( 'NONE', #16999, #4656 ) ;
#8243 = CARTESIAN_POINT ( 'NONE',  ( 158.0000000000001421, 191.4133749174225443, -45.00000000000000000 ) ) ;
#8244 = ORIENTED_EDGE ( 'NONE', *, *, #12160, .T. ) ;
#8245 = VERTEX_POINT ( 'NONE', #9486 ) ;
#8246 = VECTOR ( 'NONE', #20796, 1000.000000000000000 ) ;
#8247 = CYLINDRICAL_SURFACE ( 'NONE', #2128, 6.000000000000005329 ) ;
#8248 = ADVANCED_FACE ( 'NONE', ( #16237 ), #18241, .F. ) ;
#8249 = ORIENTED_EDGE ( 'NONE', *, *, #16395, .F. ) ;
#8250 = EDGE_CURVE ( 'NONE', #26218, #16662, #20667, .T. ) ;
#8251 = EDGE_CURVE ( 'NONE', #16577, #24145, #5437, .T. ) ;
#8252 = EDGE_LOOP ( 'NONE', ( #17748, #26898, #26108, #8107 ) ) ;
#8253 = ORIENTED_EDGE ( 'NONE', *, *, #7442, .F. ) ;
#8254 = DIRECTION ( 'NONE',  ( 0.8916010070293483025, 0.4528218681382912836, 0.000000000000000000 ) ) ;
#8255 = AXIS2_PLACEMENT_3D ( 'NONE', #23344, #18748, #21324 ) ;
#8256 = ADVANCED_FACE ( 'NONE', ( #13950 ), #2360, .T. ) ;
#8257 = DIRECTION ( 'NONE',  ( -0.8916010070293995948, -0.4528218681381900867, 0.000000000000000000 ) ) ;
#8258 = FACE_BOUND ( 'NONE', #1888, .T. ) ;
#8259 = DIRECTION ( 'NONE',  ( -0.5975062131282553590, 0.8018642810807399268, 0.000000000000000000 ) ) ;
#8260 =( BOUNDED_SURFACE ( )  B_SPLINE_SURFACE ( 3, 2, ( 
 ( #1737, #27736, #21282 ),
 ( #10514, #20862, #27451 ),
 ( #19272, #12118, #9949 ),
 ( #7794, #25310, #4175 ),
 ( #15260, #4034, #1876 ),
 ( #17537, #12964, #21715 ),
 ( #13112, #17398, #6334 ),
 ( #21993, #12822, #2446 ),
 ( #11081, #23872, #22 ),
 ( #17119, #2026, #6760 ),
 ( #19838, #2301, #24015 ),
 ( #8643, #10801, #17682 ),
 ( #26012, #4322, #15543 ),
 ( #21565, #10656, #19558 ),
 ( #17257, #4457, #28299 ),
 ( #28161, #8501, #8925 ),
 ( #11229, #15117, #24159 ),
 ( #26158, #8780, #21858 ),
 ( #2162, #26300, #14975 ),
 ( #19415, #26434, #19698 ),
 ( #6480, #10941, #6624 ),
 ( #24291, #15404, #13245 ),
 ( #163, #13385, #4600 ),
 ( #22136, #19980, #311 ),
 ( #25873, #6199, #23724 ),
 ( #22424, #20121, #11527 ),
 ( #597, #26727, #15686 ),
 ( #13824, #24437, #22572 ),
 ( #17972, #11672, #6906 ),
 ( #2736, #737, #16115 ) ),
 .UNSPECIFIED., .F., .F., .T. ) 
 B_SPLINE_SURFACE_WITH_KNOTS ( ( 4, 2, 2, 2, 2, 2, 2, 2, 2, 2, 2, 2, 2, 2, 4 ),
 ( 3, 3 ),
 ( -1.674008154317618846E-16, 0.004796186164130087151, 0.005995232705162650139, 0.007194279246195213993, 0.009592372328260340836, 0.01199046541032546681, 0.01438855849239059452, 0.01918474465652084820, 0.02158283773858597418, 0.02398093082065110015, 0.02877711698478135557, 0.03117521006684648155, 0.03357330314891161099, 0.03597139623097674044, 0.03836948931304186294 ),
 ( 0.000000000000000000, 1.000000000000000000 ),
 .UNSPECIFIED. ) 
 GEOMETRIC_REPRESENTATION_ITEM ( )  RATIONAL_B_SPLINE_SURFACE ( (
 ( 1.000000000000000000, 0.7071067811865487940, 1.000000000000000000),
 ( 1.000000000000000000, 0.7015663335576025617, 1.000000000000000000),
 ( 1.000000000000000000, 0.6988942011281563671, 1.000000000000000000),
 ( 1.000000000000000000, 0.6998716252125488646, 1.000000000000000000),
 ( 1.000000000000000000, 0.7002827442718724260, 1.000000000000000000),
 ( 1.000000000000000000, 0.7015526314445608147, 1.000000000000000000),
 ( 1.000000000000000000, 0.7024157372324350002, 1.000000000000000000),
 ( 1.000000000000000000, 0.7056510234290841455, 1.000000000000000000),
 ( 1.000000000000000000, 0.7086699596806621537, 1.000000000000000000),
 ( 1.000000000000000000, 0.7163055651782664901, 1.000000000000000000),
 ( 1.000000000000000000, 0.7209222552121633543, 1.000000000000000000),
 ( 1.000000000000000000, 0.7316018280031438836, 1.000000000000000000),
 ( 1.000000000000000000, 0.7377022142498353974, 1.000000000000000000),
 ( 1.000000000000000000, 0.7574495109011171179, 1.000000000000000000),
 ( 1.000000000000000000, 0.7725906048390918102, 1.000000000000000000),
 ( 1.000000000000000000, 0.7967368853332368328, 1.000000000000000000),
 ( 1.000000000000000000, 0.8050277828824107251, 1.000000000000000000),
 ( 1.000000000000000000, 0.8218659741008048636, 1.000000000000000000),
 ( 1.000000000000000000, 0.8303227012387988104, 1.000000000000000000),
 ( 1.000000000000000000, 0.8554219935177965750, 1.000000000000000000),
 ( 1.000000000000000000, 0.8718289199487448959, 1.000000000000000000),
 ( 1.000000000000000000, 0.8949179238641020717, 1.000000000000000000),
 ( 1.000000000000000000, 0.9023622371838861955, 1.000000000000000000),
 ( 1.000000000000000000, 0.9165667567816626615, 1.000000000000000000),
 ( 1.000000000000000000, 0.9233430263196975574, 1.000000000000000000),
 ( 1.000000000000000000, 0.9359270949453182276, 1.000000000000000000),
 ( 1.000000000000000000, 0.9416870872377598456, 1.000000000000000000),
 ( 1.000000000000000000, 0.9518583203832227113, 1.000000000000000000),
 ( 1.000000000000000000, 0.9562707360545653623, 1.000000000000000000),
 ( 1.000000000000000000, 0.9597817246759329235, 1.000000000000000000) ) ) 
 REPRESENTATION_ITEM ( '' )  SURFACE ( )  );
#8261 = CARTESIAN_POINT ( 'NONE',  ( 114.5814157129578916, 209.3660254037841923, 45.00000000000000000 ) ) ;
#8262 = AXIS2_PLACEMENT_3D ( 'NONE', #5933, #14707, #19012 ) ;
#8263 = CARTESIAN_POINT ( 'NONE',  ( 232.4999999999996305, 83.06687458711267880, 36.86484227207694175 ) ) ;
#8264 = CARTESIAN_POINT ( 'NONE',  ( -232.3551040745953458, 65.57906652092701449, -15.97735746865810214 ) ) ;
#8265 = EDGE_CURVE ( 'NONE', #25897, #10, #23930, .T. ) ;
#8266 = ORIENTED_EDGE ( 'NONE', *, *, #4124, .F. ) ;
#8267 = CARTESIAN_POINT ( 'NONE',  ( 157.9999999999998863, 216.4921249924925348, -45.00000000000000000 ) ) ;
#8268 = DIRECTION ( 'NONE',  ( 0.8916010070300282031, -0.4528218681369524101, 0.000000000000000000 ) ) ;
#8269 = CARTESIAN_POINT ( 'NONE',  ( 158.0000000000015632, 55.98812451204224061, -45.00000000000000000 ) ) ;
#8270 = CARTESIAN_POINT ( 'NONE',  ( 112.8630565061748285, 224.0572848923304718, -97.00605251950301522 ) ) ;
#8271 = EDGE_LOOP ( 'NONE', ( #16017, #15974 ) ) ;
#8272 = DIRECTION ( 'NONE',  ( 0.000000000000000000, 0.000000000000000000, -1.000000000000000000 ) ) ;
#8273 = DIRECTION ( 'NONE',  ( -0.000000000000000000, -0.000000000000000000, -1.000000000000000000 ) ) ;
#8274 = DIRECTION ( 'NONE',  ( -1.000000000000000000, 0.000000000000000000, 0.000000000000000000 ) ) ;
#8275 = CARTESIAN_POINT ( 'NONE',  ( 119.1329331941752230, 232.1752285801739220, -45.00000000000000000 ) ) ;
#8276 = CARTESIAN_POINT ( 'NONE',  ( -36.37721155344281243, 172.2515494757248291, -45.00000000000000000 ) ) ;
#8277 = EDGE_LOOP ( 'NONE', ( #13489, #25903, #7984, #19157 ) ) ;
#8278 = VECTOR ( 'NONE', #244, 1000.000000000000000 ) ;
#8279 = FACE_OUTER_BOUND ( 'NONE', #1416, .T. ) ;
#8280 = ORIENTED_EDGE ( 'NONE', *, *, #15265, .T. ) ;
#8281 = DIRECTION ( 'NONE',  ( -1.000000000000000000, 0.000000000000000000, 0.000000000000000000 ) ) ;
#8282 = ORIENTED_EDGE ( 'NONE', *, *, #6502, .T. ) ;
#8283 = ORIENTED_EDGE ( 'NONE', *, *, #5170, .F. ) ;
#8284 = CARTESIAN_POINT ( 'NONE',  ( 432.4999999999996589, 44.41075299063184190, 100.0000000000000426 ) ) ;
#8285 = VECTOR ( 'NONE', #12143, 1000.000000000000000 ) ;
#8286 = EDGE_CURVE ( 'NONE', #8829, #14508, #998, .T. ) ;
#8287 = EDGE_CURVE ( 'NONE', #10360, #1132, #10606, .T. ) ;
#8288 = EDGE_LOOP ( 'NONE', ( #20502, #9131, #27835, #4165 ) ) ;
#8289 = VERTEX_POINT ( 'NONE', #3848 ) ;
#8290 = CARTESIAN_POINT ( 'NONE',  ( 115.6411010564578561, 208.5333949360010308, 99.00000000000001421 ) ) ;
#8291 = CARTESIAN_POINT ( 'NONE',  ( -147.4641305970645533, 124.6152932964712221, -19.24112557280262692 ) ) ;
#8292 = DIRECTION ( 'NONE',  ( -0.000000000000000000, -0.000000000000000000, -1.000000000000000000 ) ) ;
#8293 = DIRECTION ( 'NONE',  ( 0.4528218681375319465, 0.8916010070297339940, -0.000000000000000000 ) ) ;
#8294 = CARTESIAN_POINT ( 'NONE',  ( 157.4999999999998579, 95.86018712840139244, 45.00000000000000000 ) ) ;
#8295 = CARTESIAN_POINT ( 'NONE',  ( 134.9999999999998579, 467.1080826427131001, -145.0000000000000000 ) ) ;
#8296 = FACE_OUTER_BOUND ( 'NONE', #13170, .T. ) ;
#8297 = CARTESIAN_POINT ( 'NONE',  ( -217.9384205093021194, 87.80450100948937120, -17.58362224480991998 ) ) ;
#8298 = EDGE_CURVE ( 'NONE', #7786, #13440, #23002, .T. ) ;
#8299 = CIRCLE ( 'NONE', #16122, 7.685040811306672381 ) ;
#8300 = EDGE_CURVE ( 'NONE', #22920, #7044, #12772, .T. ) ;
#8301 = PLANE ( 'NONE',  #7174 ) ;
#8302 = CARTESIAN_POINT ( 'NONE',  ( 157.9999999999997726, 248.5866250825770294, 45.00000000000000000 ) ) ;
#8303 = CARTESIAN_POINT ( 'NONE',  ( 157.9999999999998295, 228.5236250225210313, 45.00000000000000000 ) ) ;
#8304 = DIRECTION ( 'NONE',  ( 0.000000000000000000, 0.000000000000000000, -1.000000000000000000 ) ) ;
#8305 = FACE_OUTER_BOUND ( 'NONE', #14535, .T. ) ;
#8306 = EDGE_LOOP ( 'NONE', ( #22262, #26864, #5596, #1757 ) ) ;
#8307 = VECTOR ( 'NONE', #11169, 1000.000000000000000 ) ;
#8308 = CARTESIAN_POINT ( 'NONE',  ( 222.4999999999996021, 194.4107529906318064, -62.90796922943941638 ) ) ;
#8309 = DIRECTION ( 'NONE',  ( -0.000000000000000000, 1.000000000000000000, -1.387778780781445429E-16 ) ) ;
#8310 = CARTESIAN_POINT ( 'NONE',  ( 157.4999999999998579, 88.33656210588026170, 45.00000000000000000 ) ) ;
#8312 = ORIENTED_EDGE ( 'NONE', *, *, #8607, .F. ) ;
#8311 = ORIENTED_EDGE ( 'NONE', *, *, #10230, .F. ) ;
#8313 = ADVANCED_FACE ( 'NONE', ( #6285 ), #8164, .F. ) ;
#8314 = EDGE_CURVE ( 'NONE', #15041, #3632, #25541, .T. ) ;
#8315 = CARTESIAN_POINT ( 'NONE',  ( 93.89426149340872030, 239.9406732612796986, -18.26413231114277380 ) ) ;
#8316 = EDGE_LOOP ( 'NONE', ( #6830, #10093, #5450, #1703 ) ) ;
#8317 = ORIENTED_EDGE ( 'NONE', *, *, #13514, .T. ) ;
#8318 = ORIENTED_EDGE ( 'NONE', *, *, #21599, .F. ) ;
#8319 = TOROIDAL_SURFACE ( 'NONE', #2813, 49.99999999999999289, 30.00000000000000000 ) ;
#8320 = ORIENTED_EDGE ( 'NONE', *, *, #7076, .F. ) ;
#8321 = VERTEX_POINT ( 'NONE', #17064 ) ;
#8322 = ORIENTED_EDGE ( 'NONE', *, *, #12419, .T. ) ;
#8323 = CARTESIAN_POINT ( 'NONE',  ( 158.0000000000000000, 206.4606249624626457, -45.00000000000000000 ) ) ;
#8324 = VECTOR ( 'NONE', #2892, 1000.000000000000000 ) ;
#8325 = CARTESIAN_POINT ( 'NONE',  ( -17.24491960465747553, -23.01420295945612082, 80.00000000000001421 ) ) ;
#8326 = CARTESIAN_POINT ( 'NONE',  ( 157.4999999999998579, 146.0176872785422404, 45.00000000000000000 ) ) ;
#8327 = CARTESIAN_POINT ( 'NONE',  ( 118.0294372515226939, 235.5563491861037164, 45.00000000000000000 ) ) ;
#8328 = EDGE_CURVE ( 'NONE', #18109, #5589, #11561, .T. ) ;
#8329 = CARTESIAN_POINT ( 'NONE',  ( 157.4999999999998579, 103.3838121509225090, 45.00000000000000000 ) ) ;
#8330 = DIRECTION ( 'NONE',  ( 0.4528218681373120669, 0.8916010070298455714, -0.000000000000000000 ) ) ;
#8331 = PLANE ( 'NONE',  #10226 ) ;
#8332 = VECTOR ( 'NONE', #6947, 1000.000000000000114 ) ;
#8333 = DIRECTION ( 'NONE',  ( -0.000000000000000000, -0.000000000000000000, -1.000000000000000000 ) ) ;
#8334 = DIRECTION ( 'NONE',  ( -8.673617379884036705E-17, 1.000000000000000000, 0.000000000000000000 ) ) ;
#8335 = LINE ( 'NONE', #25851, #520 ) ;
#8336 = LINE ( 'NONE', #14526, #25801 ) ;
#8337 = AXIS2_PLACEMENT_3D ( 'NONE', #5520, #7686, #27483 ) ;
#8338 = ORIENTED_EDGE ( 'NONE', *, *, #5359, .T. ) ;
#8339 = AXIS2_PLACEMENT_3D ( 'NONE', #20888, #21305, #3497 ) ;
#8340 = CARTESIAN_POINT ( 'NONE',  ( -196.7364259845711274, 98.11380229803960162, 32.13449563926383945 ) ) ;
#8341 = TOROIDAL_SURFACE ( 'NONE', #13859, -538.1631314933625845, 562.1290781602207289 ) ;
#8342 = CARTESIAN_POINT ( 'NONE',  ( -260.0000000000001137, -167.0819201924624906, -109.9999999999998721 ) ) ;
#8343 = ORIENTED_EDGE ( 'NONE', *, *, #7217, .F. ) ;
#8344 = ITEM_DEFINED_TRANSFORMATION ( 'NONE', 'NONE', #17519,  #10637 ) ;
#8345 = ORIENTED_EDGE ( 'NONE', *, *, #10170, .F. ) ;
#8346 = EDGE_CURVE ( 'NONE', #20004, #10474, #21175, .T. ) ;
#8348 = EDGE_CURVE ( 'NONE', #12401, #88, #23679, .T. ) ;
#8347 = EDGE_LOOP ( 'NONE', ( #19447, #10257 ) ) ;
#8349 = CARTESIAN_POINT ( 'NONE',  ( 134.0000000000000853, 196.9999999999997442, -45.00000000000000000 ) ) ;
#8350 = PLANE ( 'NONE',  #6256 ) ;
#8351 = EDGE_LOOP ( 'NONE', ( #13470, #21698, #13841, #10543 ) ) ;
#8352 = EDGE_CURVE ( 'NONE', #26072, #4314, #10182, .T. ) ;
#8353 = ORIENTED_EDGE ( 'NONE', *, *, #7759, .T. ) ;
#8354 = CARTESIAN_POINT ( 'NONE',  ( 84.91648909973973502, 110.3843228243604528, -100.0000000000108571 ) ) ;
#8355 = VECTOR ( 'NONE', #28172, 1000.000000000000000 ) ;
#8356 = CARTESIAN_POINT ( 'NONE',  ( 109.9757146194093878, 258.3900549775689797, 43.60574715434479032 ) ) ;
#8357 = CARTESIAN_POINT ( 'NONE',  ( 156.9574749595459764, 213.0812361363529988, 45.00000000000000000 ) ) ;
#8358 = EDGE_LOOP ( 'NONE', ( #19886, #23578, #13452, #14559 ) ) ;
#8359 = LINE ( 'NONE', #3471, #3180 ) ;
#8360 = ORIENTED_EDGE ( 'NONE', *, *, #17601, .T. ) ;
#8361 = AXIS2_PLACEMENT_3D ( 'NONE', #13102, #28151, #19828 ) ;
#8362 = CARTESIAN_POINT ( 'NONE',  ( 158.0000000000009095, 120.6849996997183183, -45.00000000000000000 ) ) ;
#8363 = VECTOR ( 'NONE', #23783, 1000.000000000000000 ) ;
#8364 = CARTESIAN_POINT ( 'NONE',  ( 158.0000000000004547, 163.8267498348450886, -45.00000000000000000 ) ) ;
#8365 = CARTESIAN_POINT ( 'NONE',  ( 158.0000000000006821, 138.7479997597746433, 45.00000000000000000 ) ) ;
#8366 = DIRECTION ( 'NONE',  ( -0.8916010070293783896, 0.4528218681382319422, 0.000000000000000000 ) ) ;
#8367 = ORIENTED_EDGE ( 'NONE', *, *, #27725, .T. ) ;
#8368 = CARTESIAN_POINT ( 'NONE',  ( 232.4749999999995964, 83.06687458711267880, 36.86484227207694175 ) ) ;
#8369 = PLANE ( 'NONE',  #13820 ) ;
#8370 = DIRECTION ( 'NONE',  ( -0.000000000000000000, 0.000000000000000000, -1.000000000000000000 ) ) ;
#8371 = CARTESIAN_POINT ( 'NONE',  ( 124.9999999999998579, 220.0000000000000284, 45.00000000000000000 ) ) ;
#8372 = ORIENTED_EDGE ( 'NONE', *, *, #20410, .T. ) ;
#8373 = AXIS2_PLACEMENT_3D ( 'NONE', #23240, #9606, #18922 ) ;
#8374 = FACE_OUTER_BOUND ( 'NONE', #25440, .T. ) ;
#8375 = AXIS2_PLACEMENT_3D ( 'NONE', #19392, #19539, #4156 ) ;
#8376 = CARTESIAN_POINT ( 'NONE',  ( -196.7142546509254828, 98.38667968879231296, 31.27696485703440743 ) ) ;
#8377 = DIRECTION ( 'NONE',  ( 1.000000000000000000, 0.000000000000000000, -0.000000000000000000 ) ) ;
#8378 = CARTESIAN_POINT ( 'NONE',  ( -210.6527369349483081, 88.81635720432898040, 22.91843903506385871 ) ) ;
#8379 = EDGE_LOOP ( 'NONE', ( #4589, #18360, #9602, #22482 ) ) ;
#8380 =( NAMED_UNIT ( * ) PLANE_ANGLE_UNIT ( ) SI_UNIT ( $, .RADIAN. ) );
#8381 = PLANE ( 'NONE',  #20763 ) ;
#8382 = ADVANCED_FACE ( 'NONE', ( #14780 ), #8341, .T. ) ;
#8383 = VECTOR ( 'NONE', #21086, 1000.000000000000000 ) ;
#8384 = ORIENTED_EDGE ( 'NONE', *, *, #28205, .T. ) ;
#8385 = EDGE_CURVE ( 'NONE', #2973, #23432, #7007, .T. ) ;
#8386 = AXIS2_PLACEMENT_3D ( 'NONE', #22410, #9345, #10679 ) ;
#8387 = EDGE_CURVE ( 'NONE', #3645, #24118, #21046, .T. ) ;
#8388 = CARTESIAN_POINT ( 'NONE',  ( -141.7296954651576755, 126.5025729468090816, 18.19659924392545136 ) ) ;
#8389 = EDGE_CURVE ( 'NONE', #230, #23293, #19929, .T. ) ;
#8390 = CARTESIAN_POINT ( 'NONE',  ( -180.5882078327868214, 109.6574160033507468, -29.97001359623425643 ) ) ;
#8391 = ORIENTED_EDGE ( 'NONE', *, *, #23750, .T. ) ;
#8392 = ORIENTED_EDGE ( 'NONE', *, *, #13947, .T. ) ;
#8393 = LINE ( 'NONE', #17426, #20494 ) ;
#8394 = ORIENTED_EDGE ( 'NONE', *, *, #17771, .T. ) ;
#8395 = ORIENTED_EDGE ( 'NONE', *, *, #6358, .F. ) ;
#8396 = ORIENTED_EDGE ( 'NONE', *, *, #9470, .T. ) ;
#8397 = CIRCLE ( 'NONE', #8868, 1.999999999999997113 ) ;
#8398 = CARTESIAN_POINT ( 'NONE',  ( 158.0000000000013074, 83.06687458711267880, 45.00000000000000000 ) ) ;
#8399 = AXIS2_PLACEMENT_3D ( 'NONE', #26993, #11652, #20529 ) ;
#8400 = DIRECTION ( 'NONE',  ( 1.000000000000000000, 0.000000000000000000, 0.000000000000000000 ) ) ;
#8401 = PLANE ( 'NONE',  #4753 ) ;
#8402 = VECTOR ( 'NONE', #16069, 1000.000000000000000 ) ;
#8403 = CARTESIAN_POINT ( 'NONE',  ( 158.0000000000010800, 103.1298746471690038, 45.00000000000000000 ) ) ;
#8404 = DIRECTION ( 'NONE',  ( 0.000000000000000000, 0.000000000000000000, 1.000000000000000000 ) ) ;
#8405 = CARTESIAN_POINT ( 'NONE',  ( -234.0991496467425463, 66.75367139654701987, -6.159314286175092690 ) ) ;
#8406 = ORIENTED_EDGE ( 'NONE', *, *, #13779, .F. ) ;
#8407 = CARTESIAN_POINT ( 'NONE',  ( 2.016757918737201560, 1.249999999999999556, -7.548718989644206623 ) ) ;
#8408 = DIRECTION ( 'NONE',  ( 0.4528218681382693567, -0.8916010070293595158, 0.000000000000000000 ) ) ;
#8409 = CARTESIAN_POINT ( 'NONE',  ( -210.0000000000000000, -120.0000000000001705, 100.0000000000000142 ) ) ;
#8410 = DIRECTION ( 'NONE',  ( -0.8916010070293283185, -0.4528218681383305855, 0.000000000000000000 ) ) ;
#8411 = VERTEX_POINT ( 'NONE', #6853 ) ;
#8412 = CYLINDRICAL_SURFACE ( 'NONE', #3137, 5.999999999999977796 ) ;
#8413 = EDGE_CURVE ( 'NONE', #14199, #12077, #26383, .T. ) ;
#8414 = ADVANCED_FACE ( 'NONE', ( #15783 ), #3287, .T. ) ;
#8415 = CARTESIAN_POINT ( 'NONE',  ( 187.4999999999996305, 133.0668745871126930, 42.86484227207692044 ) ) ;
#8416 = DIRECTION ( 'NONE',  ( 0.4999999999999985012, 0.8660254037844394848, -0.000000000000000000 ) ) ;
#8417 = CARTESIAN_POINT ( 'NONE',  ( 232.4999999999996305, 133.0668745871126930, -36.86484227207694886 ) ) ;
#8418 = DIRECTION ( 'NONE',  ( 0.000000000000000000, -1.000000000000000000, 0.000000000000000000 ) ) ;
#8419 = DIRECTION ( 'NONE',  ( -0.000000000000000000, 0.000000000000000000, 1.000000000000000000 ) ) ;
#8420 = ORIENTED_EDGE ( 'NONE', *, *, #25002, .T. ) ;
#8421 = VECTOR ( 'NONE', #4890, 999.9999999999998863 ) ;
#8422 = ADVANCED_FACE ( 'NONE', ( #26669 ), #2251, .T. ) ;
#8423 = AXIS2_PLACEMENT_3D ( 'NONE', #9691, #11856, #18453 ) ;
#8424 = LINE ( 'NONE', #16762, #5183 ) ;
#8425 = ORIENTED_EDGE ( 'NONE', *, *, #18796, .T. ) ;
#8426 = EDGE_CURVE ( 'NONE', #14300, #16598, #538, .T. ) ;
#8427 = CYLINDRICAL_SURFACE ( 'NONE', #14496, 5.000000000000000000 ) ;
#8428 = ORIENTED_EDGE ( 'NONE', *, *, #19113, .F. ) ;
#8429 = AXIS2_PLACEMENT_3D ( 'NONE', #12275, #5506, #783 ) ;
#8430 = EDGE_LOOP ( 'NONE', ( #20900, #5407, #20480, #21730 ) ) ;
#8431 = DIRECTION ( 'NONE',  ( -0.000000000000000000, -0.000000000000000000, -1.000000000000000000 ) ) ;
#8432 = PRODUCT_DEFINITION ( 'UNKNOWN', '', #22578, #20085 ) ;
#8433 = ORIENTED_EDGE ( 'NONE', *, *, #8489, .T. ) ;
#8434 = ORIENTED_EDGE ( 'NONE', *, *, #5342, .T. ) ;
#8435 = CARTESIAN_POINT ( 'NONE',  ( -216.4421519707229606, 141.6000904446840707, 15.00000000000000000 ) ) ;
#8436 = CARTESIAN_POINT ( 'NONE',  ( -96.34017497949227504, 134.5464908775736887, -15.49978530010318956 ) ) ;
#8437 = PLANE ( 'NONE',  #17551 ) ;
#8438 = CARTESIAN_POINT ( 'NONE',  ( -151.5242873510758272, 124.1880030070812921, -19.47963555966862970 ) ) ;
#8439 = VECTOR ( 'NONE', #13009, 1000.000000000000000 ) ;
#8440 = CARTESIAN_POINT ( 'NONE',  ( -262.5386721175036655, -166.4045974903192473, -89.91974897482165829 ) ) ;
#8441 = LINE ( 'NONE', #8583, #26400 ) ;
#8442 = CARTESIAN_POINT ( 'NONE',  ( -222.3167885473197600, 86.50371922326300478, -17.61937429740468630 ) ) ;
#8443 = CARTESIAN_POINT ( 'NONE',  ( 134.9999999999998863, 250.0000000000000568, -151.0000000000000284 ) ) ;
#8444 = CARTESIAN_POINT ( 'NONE',  ( -210.0000000000000284, 59.99999999999993605, 100.0000000000000142 ) ) ;
#8445 = EDGE_CURVE ( 'NONE', #19837, #19335, #14303, .T. ) ;
#8446 = CIRCLE ( 'NONE', #17152, 7.499999999999992895 ) ;
#8447 = CARTESIAN_POINT ( 'NONE',  ( 158.0000000000015348, 60.49599951954928656, 45.00000000000000000 ) ) ;
#8448 = FACE_OUTER_BOUND ( 'NONE', #25584, .T. ) ;
#8449 = CARTESIAN_POINT ( 'NONE',  ( 158.0000000000003411, 173.8582498648732440, 45.00000000000000000 ) ) ;
#8450 = ORIENTED_EDGE ( 'NONE', *, *, #14671, .T. ) ;
#8451 = ADVANCED_FACE ( 'NONE', ( #28384 ), #13336, .F. ) ;
#8452 = FACE_OUTER_BOUND ( 'NONE', #2386, .T. ) ;
#8453 = CARTESIAN_POINT ( 'NONE',  ( 158.0000000000010516, 105.6377496546760568, -45.00000000000000000 ) ) ;
#8454 = DIRECTION ( 'NONE',  ( 0.000000000000000000, 0.000000000000000000, 1.000000000000000000 ) ) ;
#8456 = ORIENTED_EDGE ( 'NONE', *, *, #6899, .F. ) ;
#8455 = ORIENTED_EDGE ( 'NONE', *, *, #9227, .T. ) ;
#8457 = CARTESIAN_POINT ( 'NONE',  ( 106.7826897485120696, 249.1041097334270091, -25.92390487272609079 ) ) ;
#8458 = ORIENTED_EDGE ( 'NONE', *, *, #9301, .T. ) ;
#8459 = ADVANCED_FACE ( 'NONE', ( #22227 ), #2535, .F. ) ;
#8460 = ORIENTED_EDGE ( 'NONE', *, *, #12806, .T. ) ;
#8461 = ORIENTED_EDGE ( 'NONE', *, *, #25620, .T. ) ;
#8462 = ADVANCED_FACE ( 'NONE', ( #15493 ), #542, .F. ) ;
#8463 = ORIENTED_EDGE ( 'NONE', *, *, #16342, .T. ) ;
#8464 = AXIS2_PLACEMENT_3D ( 'NONE', #23455, #12699, #10529 ) ;
#8465 = ORIENTED_EDGE ( 'NONE', *, *, #12847, .F. ) ;
#8466 = ORIENTED_EDGE ( 'NONE', *, *, #15885, .T. ) ;
#8467 = DIRECTION ( 'NONE',  ( 0.000000000000000000, 0.000000000000000000, -1.000000000000000000 ) ) ;
#8468 = LINE ( 'NONE', #15082, #2725 ) ;
#8469 = DIRECTION ( 'NONE',  ( -0.7071067811865474617, -0.7071067811865474617, 0.000000000000000000 ) ) ;
#8470 = EDGE_CURVE ( 'NONE', #20045, #5588, #28049, .T. ) ;
#8471 = FACE_OUTER_BOUND ( 'NONE', #26463, .T. ) ;
#8472 = CARTESIAN_POINT ( 'NONE',  ( 158.0000000000011653, 95.60624962464788723, 45.00000000000000000 ) ) ;
#8473 = DIRECTION ( 'NONE',  ( -0.000000000000000000, -0.000000000000000000, 1.000000000000000000 ) ) ;
#8474 = CARTESIAN_POINT ( 'NONE',  ( -229.8504134091503204, 74.77134060501161628, -16.24524307967075032 ) ) ;
#8475 = VECTOR ( 'NONE', #23411, 1000.000000000000000 ) ;
#8476 = ADVANCED_FACE ( 'NONE', ( #961 ), #3387, .F. ) ;
#8477 = CARTESIAN_POINT ( 'NONE',  ( -28.13887543485015286, 129.1552015491647865, 15.69125477524985257 ) ) ;
#8478 = CARTESIAN_POINT ( 'NONE',  ( 157.4999999999998010, 233.7933125412885147, -45.00000000000000000 ) ) ;
#8479 = CARTESIAN_POINT ( 'NONE',  ( 154.8288972274760908, 222.6105238444010297, 45.00000000000000000 ) ) ;
#8480 = PLANE ( 'NONE',  #24434 ) ;
#8481 = VECTOR ( 'NONE', #13625, 1000.000000000000000 ) ;
#8482 = ORIENTED_EDGE ( 'NONE', *, *, #26274, .T. ) ;
#8483 = CARTESIAN_POINT ( 'NONE',  ( -180.3681537315997900, 109.4804799639990875, 30.93612761857035309 ) ) ;
#8484 = LINE ( 'NONE', #12808, #25480 ) ;
#8485 = ORIENTED_EDGE ( 'NONE', *, *, #15234, .F. ) ;
#8486 = VERTEX_POINT ( 'NONE', #12178 ) ;
#8487 = ORIENTED_EDGE ( 'NONE', *, *, #17597, .T. ) ;
#8488 = EDGE_CURVE ( 'NONE', #19893, #7880, #20499, .T. ) ;
#8489 = EDGE_CURVE ( 'NONE', #6964, #19653, #18490, .T. ) ;
#8490 = CARTESIAN_POINT ( 'NONE',  ( -227.8378063125350366, 130.6400894613935577, -13.00000000000000178 ) ) ;
#8491 = LINE ( 'NONE', #19405, #25513 ) ;
#8492 = VERTEX_POINT ( 'NONE', #7435 ) ;
#8493 = VECTOR ( 'NONE', #21460, 1000.000000000000000 ) ;
#8494 = VECTOR ( 'NONE', #25955, 1000.000000000000000 ) ;
#8495 = AXIS2_PLACEMENT_3D ( 'NONE', #25518, #18772, #8281 ) ;
#8496 = ORIENTED_EDGE ( 'NONE', *, *, #24657, .F. ) ;
#8497 = CARTESIAN_POINT ( 'NONE',  ( 111.0641325991587252, 99.15168937823352735, -100.0000000000000142 ) ) ;
#8498 = CARTESIAN_POINT ( 'NONE',  ( 91.02001408115319236, 230.3620936502381085, 17.09243702347552585 ) ) ;
#8499 = DIRECTION ( 'NONE',  ( 0.8916010070295820045, 0.4528218681378310406, 0.000000000000000000 ) ) ;
#8500 = ORIENTED_EDGE ( 'NONE', *, *, #25628, .F. ) ;
#8501 = CARTESIAN_POINT ( 'NONE',  ( -216.8679380397482248, 87.78479877776845797, 20.07711282125457330 ) ) ;
#8502 = EDGE_LOOP ( 'NONE', ( #7235, #22200, #27766, #10131 ) ) ;
#8503 = AXIS2_PLACEMENT_3D ( 'NONE', #26448, #6777, #20285 ) ;
#8504 = CARTESIAN_POINT ( 'NONE',  ( 232.4999999999996305, 133.0668745871126930, 42.88984227207694744 ) ) ;
#8505 = EDGE_CURVE ( 'NONE', #12774, #7618, #3244, .T. ) ;
#8506 = CARTESIAN_POINT ( 'NONE',  ( -43.02437977270766112, 129.0347155322979233, -14.93735646117640492 ) ) ;
#8507 = CARTESIAN_POINT ( 'NONE',  ( 160.8827288317913826, 204.8302013751908532, -138.9999999999999716 ) ) ;
#8508 = ADVANCED_FACE ( 'NONE', ( #22519 ), #22804, .F. ) ;
#8509 = ADVANCED_FACE ( 'NONE', ( #11897 ), #6962, .F. ) ;
#8510 = LINE ( 'NONE', #28304, #13371 ) ;
#8511 = EDGE_LOOP ( 'NONE', ( #20997, #1377 ) ) ;
#8512 = DIRECTION ( 'NONE',  ( 0.000000000000000000, 0.000000000000000000, -1.000000000000000000 ) ) ;
#8513 = AXIS2_PLACEMENT_3D ( 'NONE', #2625, #2771, #6938 ) ;
#8514 = ADVANCED_FACE ( 'NONE', ( #18213 ), #3731, .T. ) ;
#8515 = CARTESIAN_POINT ( 'NONE',  ( 134.9999999999998579, 330.0000000000000000, 84.99999999999995737 ) ) ;
#8516 = CARTESIAN_POINT ( 'NONE',  ( -13.93137870332982331, 8.043285244550061108, 45.00000000000000000 ) ) ;
#8517 = DIRECTION ( 'NONE',  ( 0.000000000000000000, -1.000000000000000000, 0.000000000000000000 ) ) ;
#8518 = AXIS2_PLACEMENT_3D ( 'NONE', #4963, #13756, #22506 ) ;
#8519 = VERTEX_POINT ( 'NONE', #4977 ) ;
#8520 = CIRCLE ( 'NONE', #24577, 30.00000000000000000 ) ;
#8521 = LINE ( 'NONE', #10816, #22470 ) ;
#8522 = CARTESIAN_POINT ( 'NONE',  ( -178.9773280279911205, 110.6332285672180120, 29.32662861827880363 ) ) ;
#8523 = CARTESIAN_POINT ( 'NONE',  ( -40.77942248602414566, 129.1863037768054596, -17.01095293969337519 ) ) ;
#8524 = DIRECTION ( 'NONE',  ( -0.000000000000000000, 0.000000000000000000, -1.000000000000000000 ) ) ;
#8525 = ORIENTED_EDGE ( 'NONE', *, *, #21147, .T. ) ;
#8526 = DIRECTION ( 'NONE',  ( 0.8916010070299369428, -0.4528218681371322663, 0.000000000000000000 ) ) ;
#8527 = AXIS2_PLACEMENT_3D ( 'NONE', #16131, #3034, #24881 ) ;
#8528 = ORIENTED_EDGE ( 'NONE', *, *, #14485, .F. ) ;
#8529 = CARTESIAN_POINT ( 'NONE',  ( 158.0000000000012790, 83.57474959461971764, 45.00000000000000000 ) ) ;
#8530 = CARTESIAN_POINT ( 'NONE',  ( -163.7479997171323305, 118.1529936970674726, -24.32116846398825416 ) ) ;
#8531 = ORIENTED_EDGE ( 'NONE', *, *, #21543, .F. ) ;
#8532 = ADVANCED_FACE ( 'NONE', ( #27372 ), #9590, .F. ) ;
#8533 = ORIENTED_EDGE ( 'NONE', *, *, #26710, .F. ) ;
#8534 = CARTESIAN_POINT ( 'NONE',  ( -71.37541315349507443, 150.2892445414773590, 5.000000000000002665 ) ) ;
#8535 = ORIENTED_EDGE ( 'NONE', *, *, #25176, .T. ) ;
#8536 = AXIS2_PLACEMENT_3D ( 'NONE', #13499, #17653, #21829 ) ;
#8537 = VERTEX_POINT ( 'NONE', #26962 ) ;
#8538 = VERTEX_POINT ( 'NONE', #24955 ) ;
#8539 = VECTOR ( 'NONE', #5941, 1000.000000000000000 ) ;
#8540 = CARTESIAN_POINT ( 'NONE',  ( 158.0000000000015632, 57.98812451204224061, -45.00000000000000000 ) ) ;
#8541 = DIRECTION ( 'NONE',  ( -0.000000000000000000, -0.000000000000000000, 1.000000000000000000 ) ) ;
#8542 = CARTESIAN_POINT ( 'NONE',  ( 157.9999999999996874, 271.1575001501400379, -45.00000000000000000 ) ) ;
#8543 = DIRECTION ( 'NONE',  ( -0.4528218681383003319, -0.8916010070293436396, 0.000000000000000000 ) ) ;
#8544 = VECTOR ( 'NONE', #15052, 1000.000000000000000 ) ;
#8545 = EDGE_CURVE ( 'NONE', #24488, #7444, #5271, .T. ) ;
#8546 = EDGE_CURVE ( 'NONE', #2404, #20577, #18435, .T. ) ;
#8547 = CARTESIAN_POINT ( 'NONE',  ( -260.0000000000001137, -167.0819201924624906, 90.00000000000001421 ) ) ;
#8548 = CARTESIAN_POINT ( 'NONE',  ( 157.9999999999997442, 251.0945000900840398, -45.00000000000000000 ) ) ;
#8549 = CARTESIAN_POINT ( 'NONE',  ( -222.1843861435924907, 71.54148064076224500, -20.10873357379266935 ) ) ;
#8550 = VERTEX_POINT ( 'NONE', #20360 ) ;
#8551 = APPLICATION_CONTEXT ( 'automotive_design' ) ;
#8552 = CARTESIAN_POINT ( 'NONE',  ( 217.4999999999996305, -5.589247009368160768, 100.0000000000000142 ) ) ;
#8553 = FACE_OUTER_BOUND ( 'NONE', #26639, .T. ) ;
#8554 = DIRECTION ( 'NONE',  ( 0.000000000000000000, -1.000000000000000000, -1.214306433183764966E-16 ) ) ;
#8555 = CARTESIAN_POINT ( 'NONE',  ( 112.8464227643157329, 215.9386697890600999, -96.99047740776124726 ) ) ;
#8556 = VERTEX_POINT ( 'NONE', #5406 ) ;
#8557 = CARTESIAN_POINT ( 'NONE',  ( -224.2511286692390513, 62.13136325095026535, 9.143584677369513969 ) ) ;
#8558 = DIRECTION ( 'NONE',  ( 1.000000000000000000, 0.000000000000000000, 0.000000000000000000 ) ) ;
#8559 = DIRECTION ( 'NONE',  ( -1.000000000000000000, 0.000000000000000000, 0.000000000000000000 ) ) ;
#8560 = DIRECTION ( 'NONE',  ( 0.4528218681374507892, -0.8916010070297751833, 0.000000000000000000 ) ) ;
#8561 = DIRECTION ( 'NONE',  ( -0.8916010070298360235, -0.4528218681373308852, 0.000000000000000000 ) ) ;
#8562 = ORIENTED_EDGE ( 'NONE', *, *, #27241, .F. ) ;
#8563 = VECTOR ( 'NONE', #21352, 1000.000000000000000 ) ;
#8564 = CARTESIAN_POINT ( 'NONE',  ( -235.6754299164472854, 80.57958899222390414, 15.03010587785140650 ) ) ;
#8565 = VERTEX_POINT ( 'NONE', #14186 ) ;
#8566 = CARTESIAN_POINT ( 'NONE',  ( -261.6207973860045968, -166.7238599877898935, 110.0000000000000142 ) ) ;
#8567 = ORIENTED_EDGE ( 'NONE', *, *, #26142, .T. ) ;
#8568 = AXIS2_PLACEMENT_3D ( 'NONE', #530, #7704, #18203 ) ;
#8569 = ORIENTED_EDGE ( 'NONE', *, *, #23557, .T. ) ;
#8570 = LINE ( 'NONE', #6549, #1661 ) ;
#8571 = EDGE_CURVE ( 'NONE', #16727, #12559, #22100, .T. ) ;
#8572 = ORIENTED_EDGE ( 'NONE', *, *, #5268, .F. ) ;
#8573 = ORIENTED_EDGE ( 'NONE', *, *, #11750, .F. ) ;
#8574 = CARTESIAN_POINT ( 'NONE',  ( 158.0000000000004263, 168.3346248423521274, 45.00000000000000000 ) ) ;
#8575 = DIRECTION ( 'NONE',  ( 1.000000000000000000, 0.000000000000000000, 0.000000000000000000 ) ) ;
#8576 = PLANE ( 'NONE',  #5177 ) ;
#8577 = CARTESIAN_POINT ( 'NONE',  ( 48.45469728424487244, 192.9461374953035033, 15.00000000000000000 ) ) ;
#8578 = EDGE_CURVE ( 'NONE', #16577, #18911, #22939, .T. ) ;
#8579 = FACE_OUTER_BOUND ( 'NONE', #22839, .T. ) ;
#8580 = AXIS2_PLACEMENT_3D ( 'NONE', #2471, #15006, #23755 ) ;
#8581 = ADVANCED_FACE ( 'NONE', ( #18767 ), #24817, .F. ) ;
#8582 = CARTESIAN_POINT ( 'NONE',  ( -261.1919288306252724, -171.9377729149742038, -89.99999999999987210 ) ) ;
#8583 = CARTESIAN_POINT ( 'NONE',  ( 79.99999999999992895, 240.0000000000000284, 5.000000000000002665 ) ) ;
#8584 = CARTESIAN_POINT ( 'NONE',  ( -219.8865548899133842, 87.95092811395369381, -16.46640705182500497 ) ) ;
#8585 = ADVANCED_FACE ( 'NONE', ( #9867, #18625 ), #5550, .F. ) ;
#8586 = DIRECTION ( 'NONE',  ( 1.000000000000000000, -0.000000000000000000, -0.000000000000000000 ) ) ;
#8587 = CARTESIAN_POINT ( 'NONE',  ( 134.9999999999998579, 220.0000000000000284, -169.9999999999999716 ) ) ;
#8588 = DIRECTION ( 'NONE',  ( -0.000000000000000000, 0.000000000000000000, -1.000000000000000000 ) ) ;
#8589 = CARTESIAN_POINT ( 'NONE',  ( 157.9999999999996589, 276.6811251726610976, -45.00000000000000000 ) ) ;
#8590 = DIRECTION ( 'NONE',  ( 0.8916010070297338830, -0.4528218681375318910, 0.000000000000000000 ) ) ;
#8591 = ORIENTED_EDGE ( 'NONE', *, *, #9752, .F. ) ;
#8592 = DIRECTION ( 'NONE',  ( 0.000000000000000000, 0.000000000000000000, -1.000000000000000000 ) ) ;
#8593 = CARTESIAN_POINT ( 'NONE',  ( 156.5461074670752453, 207.5603490538953224, -145.0000000000000000 ) ) ;
#8594 = CARTESIAN_POINT ( 'NONE',  ( 157.4999999999998579, 148.5255622860493077, -45.00000000000000000 ) ) ;
#8595 = DIRECTION ( 'NONE',  ( 0.8916010070294706491, 0.4528218681380502542, 0.000000000000000000 ) ) ;
#8596 = ORIENTED_EDGE ( 'NONE', *, *, #24179, .F. ) ;
#8597 = CARTESIAN_POINT ( 'NONE',  ( 106.7420202941123080, 244.4253804639438670, -31.38183343148740789 ) ) ;
#8598 = ORIENTED_EDGE ( 'NONE', *, *, #15070, .F. ) ;
#8599 = DIRECTION ( 'NONE',  ( 1.000000000000000000, 2.602085213965211135E-16, -0.000000000000000000 ) ) ;
#8600 = ORIENTED_EDGE ( 'NONE', *, *, #9379, .F. ) ;
#8601 = AXIS2_PLACEMENT_3D ( 'NONE', #23867, #17, #8777 ) ;
#8602 = ORIENTED_EDGE ( 'NONE', *, *, #24281, .F. ) ;
#8603 = ORIENTED_EDGE ( 'NONE', *, *, #19756, .F. ) ;
#8604 = ORIENTED_EDGE ( 'NONE', *, *, #26964, .F. ) ;
#8605 = ORIENTED_EDGE ( 'NONE', *, *, #13093, .T. ) ;
#8606 = CARTESIAN_POINT ( 'NONE',  ( -17.24491960465745777, 24.64876300893806160, 95.00000000000000000 ) ) ;
#8607 = EDGE_CURVE ( 'NONE', #20671, #16796, #19184, .T. ) ;
#8608 = PLANE ( 'NONE',  #3190 ) ;
#8609 = PRODUCT_DEFINITION_CONTEXT ( 'detailed design', #10391, 'design' ) ;
#8610 = DIRECTION ( 'NONE',  ( 0.000000000000000000, -1.000000000000000000, 0.000000000000000000 ) ) ;
#8612 = CIRCLE ( 'NONE', #4926, 21.49999999999999289 ) ;
#8611 = DIRECTION ( 'NONE',  ( -0.000000000000000000, -0.000000000000000000, -1.000000000000000000 ) ) ;
#8613 = DIRECTION ( 'NONE',  ( 1.000000000000000000, -0.000000000000000000, -0.000000000000000000 ) ) ;
#8614 = EDGE_CURVE ( 'NONE', #27410, #729, #21624, .T. ) ;
#8615 = CARTESIAN_POINT ( 'NONE',  ( 158.0000000000011369, 98.11412463215494029, -45.00000000000000000 ) ) ;
#8616 = LINE ( 'NONE', #11055, #12163 ) ;
#8617 = LINE ( 'NONE', #17368, #375 ) ;
#8618 = AXIS2_PLACEMENT_3D ( 'NONE', #10024, #9605, #3257 ) ;
#8619 = DIRECTION ( 'NONE',  ( 0.000000000000000000, 0.000000000000000000, 1.000000000000000000 ) ) ;
#8620 = ADVANCED_FACE ( 'NONE', ( #28075 ), #25511, .F. ) ;
#8621 = FACE_OUTER_BOUND ( 'NONE', #5014, .T. ) ;
#8622 = CARTESIAN_POINT ( 'NONE',  ( 158.0000000000001421, 191.4133749174225443, 45.00000000000000000 ) ) ;
#8623 = DIRECTION ( 'NONE',  ( 1.000000000000000000, -0.000000000000000000, -0.000000000000000000 ) ) ;
#8624 = CARTESIAN_POINT ( 'NONE',  ( 157.9999999999996589, 278.6811251726610976, -45.00000000000000000 ) ) ;
#8626 = VERTEX_POINT ( 'NONE', #19328 ) ;
#8625 = VERTEX_POINT ( 'NONE', #21059 ) ;
#8627 = CARTESIAN_POINT ( 'NONE',  ( -233.2943309833541718, 92.06151970357193193, -15.00000000000000000 ) ) ;
#8628 = CARTESIAN_POINT ( 'NONE',  ( -261.1919288306253293, -171.9377729149742038, -104.9999999999998721 ) ) ;
#8629 = VERTEX_POINT ( 'NONE', #12879 ) ;
#8630 = APPLICATION_PROTOCOL_DEFINITION ( 'draft international standard', 'automotive_design', 1998, #3578 ) ;
#8631 = EDGE_LOOP ( 'NONE', ( #12437, #22640, #8849, #22868 ) ) ;
#8632 = ORIENTED_EDGE ( 'NONE', *, *, #20283, .T. ) ;
#8633 = VECTOR ( 'NONE', #8158, 1000.000000000000114 ) ;
#8634 = CARTESIAN_POINT ( 'NONE',  ( -224.0246150495856625, 134.1142769380917912, -12.98324324876687719 ) ) ;
#8635 = DIRECTION ( 'NONE',  ( 0.000000000000000000, 0.000000000000000000, -1.000000000000000000 ) ) ;
#8636 = B_SPLINE_CURVE_WITH_KNOTS ( 'NONE', 3,
 ( #24070, #2211, #72, #8834, #6678, #15456, #22629, #9415, #15743, #11136, #7399, #2496, #24490, #11578, #26930, #19891, #5232, #7108, #4650, #16166, #4799, #361, #13586, #13732 ),
 .UNSPECIFIED., .F., .F.,
 ( 4, 2, 2, 2, 2, 2, 2, 2, 2, 2, 2, 4 ),
 ( 0.000000000000000000, 0.005230979107866756510, 0.01046195821573351302, 0.01307744776966689344, 0.01569293732360027213, 0.02092391643146711971, 0.02353940598540057300, 0.02615489553933402281, 0.03138587464720085651, 0.03400136420113424041, 0.03661685375506761042, 0.04184783286293437127 ),
 .UNSPECIFIED. ) ;
#8637 = VECTOR ( 'NONE', #18306, 1000.000000000000114 ) ;
#8638 = ORIENTED_EDGE ( 'NONE', *, *, #15780, .F. ) ;
#8639 = CARTESIAN_POINT ( 'NONE',  ( 109.9999999999999432, 140.0000000000000000, -100.0000000000000142 ) ) ;
#8640 = EDGE_CURVE ( 'NONE', #21329, #24666, #18905, .T. ) ;
#8641 = CARTESIAN_POINT ( 'NONE',  ( -178.8341066938216386, 110.7300218161632444, -29.28299286780852029 ) ) ;
#8642 = EDGE_LOOP ( 'NONE', ( #24380, #20477, #27828, #15741 ) ) ;
#8643 = CARTESIAN_POINT ( 'NONE',  ( -223.0240206785557859, 86.63361387472085084, 17.31476664850702107 ) ) ;
#8644 = ORIENTED_EDGE ( 'NONE', *, *, #18445, .T. ) ;
#8645 = LINE ( 'NONE', #26580, #5211 ) ;
#8646 = DIRECTION ( 'NONE',  ( 6.123233995736667428E-17, -1.060575238724912585E-16, -1.000000000000000000 ) ) ;
#8647 = CARTESIAN_POINT ( 'NONE',  ( 65.00000000000000000, -170.0000000000000853, -69.99999999999998579 ) ) ;
#8648 = DIRECTION ( 'NONE',  ( 0.000000000000000000, -0.000000000000000000, 1.000000000000000000 ) ) ;
#8649 = AXIS2_PLACEMENT_3D ( 'NONE', #24102, #17058, #25817 ) ;
#8650 = VERTEX_POINT ( 'NONE', #5696 ) ;
#8651 = EDGE_CURVE ( 'NONE', #18634, #22236, #23502, .T. ) ;
#8652 = EDGE_CURVE ( 'NONE', #15612, #19228, #19472, .T. ) ;
#8653 = DIRECTION ( 'NONE',  ( 0.4528218681382713551, -0.8916010070293584056, 0.000000000000000000 ) ) ;
#8654 = VECTOR ( 'NONE', #637, 1000.000000000000000 ) ;
#8655 = CARTESIAN_POINT ( 'NONE',  ( 232.4999999999996305, 83.06687458711267880, -36.86484227207694175 ) ) ;
#8656 = DIRECTION ( 'NONE',  ( 2.775557561562887407E-16, 3.668437989309015303E-32, 1.000000000000000000 ) ) ;
#8657 = CARTESIAN_POINT ( 'NONE',  ( 157.4999999999998579, 178.6200623761337738, 45.00000000000000000 ) ) ;
#8658 = ORIENTED_EDGE ( 'NONE', *, *, #24700, .F. ) ;
#8659 = CARTESIAN_POINT ( 'NONE',  ( -211.9745545450854536, -220.0000000000000853, -106.5998536507705552 ) ) ;
#8660 = CARTESIAN_POINT ( 'NONE',  ( -162.7087466801204698, 119.3764571194343915, 22.15020238234947669 ) ) ;
#8661 = CARTESIAN_POINT ( 'NONE',  ( -214.1043220540802565, 88.03185359167697754, 20.18450238099627825 ) ) ;
#8662 = ORIENTED_EDGE ( 'NONE', *, *, #9300, .F. ) ;
#8663 = ORIENTED_EDGE ( 'NONE', *, *, #445, .T. ) ;
#8664 = ADVANCED_FACE ( 'NONE', ( #3527 ), #13883, .T. ) ;
#8665 = ADVANCED_FACE ( 'NONE', ( #25790 ), #1659, .T. ) ;
#8666 = CARTESIAN_POINT ( 'NONE',  ( -215.4886702565632106, 139.8420026707766226, 12.99999999999999822 ) ) ;
#8667 = VECTOR ( 'NONE', #22291, 1000.000000000000000 ) ;
#8668 = CARTESIAN_POINT ( 'NONE',  ( -186.8676103567957227, 105.5662940401322629, -31.69060553503991073 ) ) ;
#8669 = VERTEX_POINT ( 'NONE', #6117 ) ;
#8670 = ORIENTED_EDGE ( 'NONE', *, *, #23217, .T. ) ;
#8671 = DIRECTION ( 'NONE',  ( -1.000000000000000000, 0.000000000000000000, 0.000000000000000000 ) ) ;
#8672 = VECTOR ( 'NONE', #8971, 1000.000000000000000 ) ;
#8673 = CARTESIAN_POINT ( 'NONE',  ( 158.0000000000013642, 78.05112457209858690, 45.00000000000000000 ) ) ;
#8674 = AXIS2_PLACEMENT_3D ( 'NONE', #3868, #8330, #1155 ) ;
#8675 = EDGE_CURVE ( 'NONE', #12396, #6070, #12459, .T. ) ;
#8676 = ORIENTED_EDGE ( 'NONE', *, *, #6653, .F. ) ;
#8677 = VERTEX_POINT ( 'NONE', #21480 ) ;
#8678 = FACE_BOUND ( 'NONE', #4061, .T. ) ;
#8679 = VECTOR ( 'NONE', #25037, 1000.000000000000000 ) ;
#8680 = CARTESIAN_POINT ( 'NONE',  ( 162.0806940948679085, 180.4841764145329250, 45.00000000000000000 ) ) ;
#8681 = FACE_OUTER_BOUND ( 'NONE', #5238, .T. ) ;
#8682 = LINE ( 'NONE', #1918, #14947 ) ;
#8683 = FACE_OUTER_BOUND ( 'NONE', #24848, .T. ) ;
#8684 = LINE ( 'NONE', #6801, #2245 ) ;
#8685 = ORIENTED_EDGE ( 'NONE', *, *, #11674, .F. ) ;
#8686 = AXIS2_PLACEMENT_3D ( 'NONE', #8693, #20026, #24202 ) ;
#8687 = CARTESIAN_POINT ( 'NONE',  ( 158.0000000000003979, 170.8424998498591663, 45.00000000000000000 ) ) ;
#8688 = AXIS2_PLACEMENT_3D ( 'NONE', #18845, #23018, #12542 ) ;
#8689 = CARTESIAN_POINT ( 'NONE',  ( 158.0000000000002274, 185.8897498949014278, -45.00000000000000000 ) ) ;
#8690 = CARTESIAN_POINT ( 'NONE',  ( 158.0000000000001137, 195.9212499249295831, -45.00000000000000000 ) ) ;
#8691 = DIRECTION ( 'NONE',  ( -0.8916010070293383105, -0.4528218681383106015, 0.000000000000000000 ) ) ;
#8692 = ORIENTED_EDGE ( 'NONE', *, *, #8385, .F. ) ;
#8693 = CARTESIAN_POINT ( 'NONE',  ( 158.0000000000013358, 78.55899957960562574, 45.00000000000000000 ) ) ;
#8694 = AXIS2_PLACEMENT_3D ( 'NONE', #15061, #2249, #22083 ) ;
#8695 = LINE ( 'NONE', #22191, #21703 ) ;
#8696 = CARTESIAN_POINT ( 'NONE',  ( -210.0000000000000000, -150.0000000000002558, 100.0000000000000142 ) ) ;
#8697 = DIRECTION ( 'NONE',  ( 0.8916010070296834789, 0.4528218681376311450, 0.000000000000000000 ) ) ;
#8698 = LINE ( 'NONE', #10716, #12925 ) ;
#8699 = CARTESIAN_POINT ( 'NONE',  ( -112.3221550338875687, 17.24192588826928585, 83.00000000000001421 ) ) ;
#8700 = ORIENTED_EDGE ( 'NONE', *, *, #11905, .T. ) ;
#8701 = CARTESIAN_POINT ( 'NONE',  ( -226.4422656491013299, 72.85741102083747478, 17.64402269315965910 ) ) ;
#8702 = ORIENTED_EDGE ( 'NONE', *, *, #14087, .F. ) ;
#8703 = PLANE ( 'NONE',  #2088 ) ;
#8704 = EDGE_LOOP ( 'NONE', ( #16486, #22487, #6406, #3568 ) ) ;
#8705 = VERTEX_POINT ( 'NONE', #10572 ) ;
#8706 = EDGE_CURVE ( 'NONE', #11442, #15969, #28219, .T. ) ;
#8707 = LINE ( 'NONE', #13175, #3481 ) ;
#8708 = AXIS2_PLACEMENT_3D ( 'NONE', #28175, #4336, #4469 ) ;
#8709 = ADVANCED_FACE ( 'NONE', ( #25931 ), #2841, .T. ) ;
#8710 = ORIENTED_EDGE ( 'NONE', *, *, #4178, .F. ) ;
#8711 = ORIENTED_EDGE ( 'NONE', *, *, #13486, .T. ) ;
#8712 = FACE_OUTER_BOUND ( 'NONE', #20959, .T. ) ;
#8713 = CARTESIAN_POINT ( 'NONE',  ( 158.0000000000011369, 96.11412463215494029, 45.00000000000000000 ) ) ;
#8714 = CARTESIAN_POINT ( 'NONE',  ( -213.1553235149935119, -216.8625818770119338, 94.90660418304274515 ) ) ;
#8715 = CIRCLE ( 'NONE', #1907, 49.99999999999998579 ) ;
#8716 = CARTESIAN_POINT ( 'NONE',  ( -160.0000000000000284, 59.99999999999994316, 110.0000000000000284 ) ) ;
#8717 = FACE_OUTER_BOUND ( 'NONE', #9079, .T. ) ;
#8718 = CARTESIAN_POINT ( 'NONE',  ( -175.0000000000000000, -150.0000000000000853, 76.00000000000001421 ) ) ;
#8719 = PLANE ( 'NONE',  #8039 ) ;
#8720 = CARTESIAN_POINT ( 'NONE',  ( -215.3975081536182756, 87.85043416605050481, -19.22867602304995671 ) ) ;
#8721 = LINE ( 'NONE', #9005, #20015 ) ;
#8722 = CARTESIAN_POINT ( 'NONE',  ( 157.4999999999998579, 130.9704372334999789, 45.00000000000000000 ) ) ;
#8723 = FACE_OUTER_BOUND ( 'NONE', #18667, .T. ) ;
#8724 = DIRECTION ( 'NONE',  ( -0.000000000000000000, -0.000000000000000000, -1.000000000000000000 ) ) ;
#8725 = LINE ( 'NONE', #6426, #17131 ) ;
#8726 = ORIENTED_EDGE ( 'NONE', *, *, #1540, .T. ) ;
#8727 = CARTESIAN_POINT ( 'NONE',  ( 151.9705627484769650, 235.5563491861038017, 45.00000000000000000 ) ) ;
#8728 = AXIS2_PLACEMENT_3D ( 'NONE', #14309, #17331, #12759 ) ;
#8729 = EDGE_CURVE ( 'NONE', #26896, #11940, #6254, .T. ) ;
#8730 = DIRECTION ( 'NONE',  ( 0.8706753206611566043, 0.000000000000000000, -0.4918581970360891842 ) ) ;
#8731 = CARTESIAN_POINT ( 'NONE',  ( 157.4999999999998579, 55.73418700828869277, 45.00000000000000000 ) ) ;
#8732 = CARTESIAN_POINT ( 'NONE',  ( 157.4999999999998579, 73.28931206083800021, 45.00000000000000000 ) ) ;
#8733 = ORIENTED_EDGE ( 'NONE', *, *, #20852, .F. ) ;
#8734 = AXIS2_PLACEMENT_3D ( 'NONE', #6303, #21396, #10769 ) ;
#8735 = CARTESIAN_POINT ( 'NONE',  ( 99.67744569821567779, 242.4823527582474014, -13.37113024292605878 ) ) ;
#8736 = ORIENTED_EDGE ( 'NONE', *, *, #3737, .T. ) ;
#8737 = CARTESIAN_POINT ( 'NONE',  ( -40.35451784973074751, 130.4209458812801756, -15.14568436839074117 ) ) ;
#8738 = ORIENTED_EDGE ( 'NONE', *, *, #21569, .T. ) ;
#8739 = EDGE_CURVE ( 'NONE', #7910, #5416, #1384, .T. ) ;
#8740 = ORIENTED_EDGE ( 'NONE', *, *, #13712, .T. ) ;
#8741 = EDGE_CURVE ( 'NONE', #5416, #152, #7991, .T. ) ;
#8742 = EDGE_CURVE ( 'NONE', #21276, #21518, #23357, .T. ) ;
#8743 = EDGE_CURVE ( 'NONE', #19998, #24464, #8132, .T. ) ;
#8744 = ORIENTED_EDGE ( 'NONE', *, *, #4227, .T. ) ;
#8745 = ORIENTED_EDGE ( 'NONE', *, *, #16955, .T. ) ;
#8746 = CARTESIAN_POINT ( 'NONE',  ( 115.6411010564592061, 231.4666050640012998, 99.00000000000001421 ) ) ;
#8747 = PLANE ( 'NONE',  #2164 ) ;
#8748 = VECTOR ( 'NONE', #1508, 1000.000000000000000 ) ;
#8749 = DIRECTION ( 'NONE',  ( 0.000000000000000000, 0.000000000000000000, -1.000000000000000000 ) ) ;
#8750 = CARTESIAN_POINT ( 'NONE',  ( 157.9999999999997158, 261.1260001201120531, -45.00000000000000000 ) ) ;
#8751 = VECTOR ( 'NONE', #14944, 1000.000000000000000 ) ;
#8752 = CARTESIAN_POINT ( 'NONE',  ( -215.0107612850210899, 71.82996193033663701, 26.64107447012230878 ) ) ;
#8753 = CARTESIAN_POINT ( 'NONE',  ( 137.6105238444007455, 239.8288972274759203, 45.00000000000000000 ) ) ;
#8754 = DIRECTION ( 'NONE',  ( 1.000000000000000000, 0.000000000000000000, -0.000000000000000000 ) ) ;
#8755 = CARTESIAN_POINT ( 'NONE',  ( 134.9999999999998579, 171.5103103742661688, -84.99999999999997158 ) ) ;
#8756 = DIRECTION ( 'NONE',  ( -0.000000000000000000, -0.000000000000000000, -1.000000000000000000 ) ) ;
#8757 = CYLINDRICAL_SURFACE ( 'NONE', #3103, 67.21503689626328537 ) ;
#8758 = CARTESIAN_POINT ( 'NONE',  ( 33.10302365956999182, 203.2034914284457159, -15.00000000000000000 ) ) ;
#8759 = CARTESIAN_POINT ( 'NONE',  ( 109.4209008705013417, 204.3200822355380240, -150.9609010065648818 ) ) ;
#8760 = DIRECTION ( 'NONE',  ( -0.8916010070293484135, 0.4528218681382909505, 0.000000000000000000 ) ) ;
#8761 = LINE ( 'NONE', #13656, #17962 ) ;
#8762 = DIRECTION ( 'NONE',  ( -0.8916010070290389944, 0.4528218681389001299, 0.000000000000000000 ) ) ;
#8764 = VERTEX_POINT ( 'NONE', #4376 ) ;
#8763 = ORIENTED_EDGE ( 'NONE', *, *, #11750, .T. ) ;
#8765 = CARTESIAN_POINT ( 'NONE',  ( -160.5161435040798779, 120.3804527765386752, 22.28951900308573286 ) ) ;
#8766 = EDGE_CURVE ( 'NONE', #2485, #1653, #15601, .T. ) ;
#8767 = VECTOR ( 'NONE', #13649, 1000.000000000000000 ) ;
#8768 = DIRECTION ( 'NONE',  ( 1.000000000000000000, -0.000000000000000000, -0.000000000000000000 ) ) ;
#8769 = ORIENTED_EDGE ( 'NONE', *, *, #3961, .T. ) ;
#8770 = ORIENTED_EDGE ( 'NONE', *, *, #4874, .T. ) ;
#8771 = VERTEX_POINT ( 'NONE', #13165 ) ;
#8772 = VECTOR ( 'NONE', #24559, 1000.000000000000114 ) ;
#8773 = DIRECTION ( 'NONE',  ( 1.000000000000000000, 0.000000000000000000, 0.000000000000000000 ) ) ;
#8774 = CARTESIAN_POINT ( 'NONE',  ( -273.6211430000234373, -91.18033988749901653, 0.000000000000000000 ) ) ;
#8775 = EDGE_CURVE ( 'NONE', #10126, #18558, #2499, .T. ) ;
#8776 = VERTEX_POINT ( 'NONE', #24073 ) ;
#8777 = DIRECTION ( 'NONE',  ( 0.000000000000000000, 1.000000000000000000, 0.000000000000000000 ) ) ;
#8778 = LINE ( 'NONE', #26298, #25204 ) ;
#8779 = VERTEX_POINT ( 'NONE', #4654 ) ;
#8780 = CARTESIAN_POINT ( 'NONE',  ( -214.9847395972752508, 87.90486964456984254, 21.25064676488950255 ) ) ;
#8781 = LINE ( 'NONE', #17684, #8887 ) ;
#8782 = AXIS2_PLACEMENT_3D ( 'NONE', #26095, #21226, #13054 ) ;
#8783 = CYLINDRICAL_SURFACE ( 'NONE', #24513, 7.499999999999992895 ) ;
#8784 = CARTESIAN_POINT ( 'NONE',  ( 159.5478513586114389, 202.7507791982433787, -150.3903514073974179 ) ) ;
#8785 = VECTOR ( 'NONE', #15600, 1000.000000000000000 ) ;
#8786 = VECTOR ( 'NONE', #20099, 999.9999999999998863 ) ;
#8787 = ORIENTED_EDGE ( 'NONE', *, *, #13546, .F. ) ;
#8788 = LINE ( 'NONE', #17265, #6326 ) ;
#8789 = DIRECTION ( 'NONE',  ( 0.8916010070293383105, -0.4528218681383106015, 0.000000000000000000 ) ) ;
#8790 = PLANE ( 'NONE',  #3772 ) ;
#8791 = LINE ( 'NONE', #13691, #4312 ) ;
#8792 = EDGE_LOOP ( 'NONE', ( #21299, #20133, #23187, #12749 ) ) ;
#8793 = CARTESIAN_POINT ( 'NONE',  ( -211.5426265866423989, -220.0000000000000853, -107.5190003421799645 ) ) ;
#8794 = EDGE_CURVE ( 'NONE', #22498, #12331, #20033, .T. ) ;
#8795 = LINE ( 'NONE', #22153, #26252 ) ;
#8796 = LINE ( 'NONE', #11393, #19517 ) ;
#8797 = VERTEX_POINT ( 'NONE', #15320 ) ;
#8798 = VERTEX_POINT ( 'NONE', #17594 ) ;
#8799 = VECTOR ( 'NONE', #22472, 1000.000000000000000 ) ;
#8800 = MANIFOLD_SOLID_BREP ( '\X2\00d8\X0\12.0mm Dowel Hole2[2]', #7685 ) ;
#8801 = LINE ( 'NONE', #13553, #12941 ) ;
#8802 = CARTESIAN_POINT ( 'NONE',  ( -192.2959713312834538, 101.7311354626386333, -32.42984626233510426 ) ) ;
#8803 = ORIENTED_EDGE ( 'NONE', *, *, #6323, .F. ) ;
#8804 = VECTOR ( 'NONE', #22595, 1000.000000000000000 ) ;
#8805 = ORIENTED_EDGE ( 'NONE', *, *, #26998, .F. ) ;
#8806 = FACE_OUTER_BOUND ( 'NONE', #9492, .T. ) ;
#8807 = EDGE_CURVE ( 'NONE', #12519, #26013, #6959, .T. ) ;
#8808 = DIRECTION ( 'NONE',  ( 0.4528218681380715149, 0.8916010070294598799, -0.000000000000000000 ) ) ;
#8809 = EDGE_CURVE ( 'NONE', #606, #26119, #17522, .T. ) ;
#8810 = ORIENTED_EDGE ( 'NONE', *, *, #10328, .F. ) ;
#8811 = VERTEX_POINT ( 'NONE', #2649 ) ;
#8812 = DIRECTION ( 'NONE',  ( -0.7892793597178168197, -0.6140342761796225846, 2.738362868812879575E-15 ) ) ;
#8813 = DIRECTION ( 'NONE',  ( -0.8916010070299577039, -0.4528218681370910215, 0.000000000000000000 ) ) ;
#8814 = PLANE ( 'NONE',  #3854 ) ;
#8815 = CARTESIAN_POINT ( 'NONE',  ( 157.4999999999998579, 118.4310621959647563, -45.00000000000000000 ) ) ;
#8816 = CARTESIAN_POINT ( 'NONE',  ( 157.9999999999998295, 229.0315000300280417, -45.00000000000000000 ) ) ;
#8817 = EDGE_CURVE ( 'NONE', #16274, #23832, #11435, .T. ) ;
#8818 = VECTOR ( 'NONE', #14542, 1000.000000000000000 ) ;
#8819 = CARTESIAN_POINT ( 'NONE',  ( 134.9999999999998579, 220.0000000000000284, -122.9999999999999574 ) ) ;
#8820 = CARTESIAN_POINT ( 'NONE',  ( -175.0000000000000000, -120.0000000000001705, 76.02500000000001990 ) ) ;
#8821 = ORIENTED_EDGE ( 'NONE', *, *, #17771, .F. ) ;
#8822 = EDGE_CURVE ( 'NONE', #22331, #13033, #9747, .T. ) ;
#8823 = AXIS2_PLACEMENT_3D ( 'NONE', #25563, #1582, #12664 ) ;
#8824 = CARTESIAN_POINT ( 'NONE',  ( 157.4999999999998579, 141.0019372635281627, -45.00000000000000000 ) ) ;
#8825 = DIRECTION ( 'NONE',  ( -0.000000000000000000, -0.000000000000000000, -1.000000000000000000 ) ) ;
#8827 = LINE ( 'NONE', #5964, #5446 ) ;
#8826 = AXIS2_PLACEMENT_3D ( 'NONE', #16467, #22653, #5258 ) ;
#8828 = LINE ( 'NONE', #17729, #2456 ) ;
#8829 = VERTEX_POINT ( 'NONE', #8699 ) ;
#8830 = CARTESIAN_POINT ( 'NONE',  ( 158.0000000000015064, 63.00387452705633251, 45.00000000000000000 ) ) ;
#8831 = VECTOR ( 'NONE', #14156, 1000.000000000000114 ) ;
#8832 = ORIENTED_EDGE ( 'NONE', *, *, #27000, .F. ) ;
#8833 = DIRECTION ( 'NONE',  ( 0.8660254037844394848, -0.4999999999999985012, 0.000000000000000000 ) ) ;
#8834 = CARTESIAN_POINT ( 'NONE',  ( -239.7229382034104788, 70.94047833162919403, -5.249966640536483986 ) ) ;
#8835 = CARTESIAN_POINT ( 'NONE',  ( -260.0000000000001137, -165.0000000000001137, -59.99999999999986500 ) ) ;
#8836 = CARTESIAN_POINT ( 'NONE',  ( -68.57415822541635464, -23.01420295945612082, 80.00000000000001421 ) ) ;
#8837 = FILL_AREA_STYLE ('',( #4514 ) ) ;
#8838 = ORIENTED_EDGE ( 'NONE', *, *, #3141, .T. ) ;
#8839 = CARTESIAN_POINT ( 'NONE',  ( -227.7492452350401493, 73.49917159638472697, 17.05328293002254014 ) ) ;
#8840 = ORIENTED_EDGE ( 'NONE', *, *, #2019, .T. ) ;
#8841 = DIRECTION ( 'NONE',  ( 0.000000000000000000, -1.000000000000000000, 0.000000000000000000 ) ) ;
#8842 = ORIENTED_EDGE ( 'NONE', *, *, #15827, .T. ) ;
#8843 = CIRCLE ( 'NONE', #26722, 5.000000000000004441 ) ;
#8844 = ORIENTED_EDGE ( 'NONE', *, *, #14697, .F. ) ;
#8845 = EDGE_CURVE ( 'NONE', #2445, #17060, #17452, .T. ) ;
#8846 = CARTESIAN_POINT ( 'NONE',  ( 158.0000000000001990, 186.3976249024084666, 45.00000000000000000 ) ) ;
#8847 = EDGE_CURVE ( 'NONE', #20391, #27472, #2214, .T. ) ;
#8848 = VECTOR ( 'NONE', #2717, 1000.000000000000000 ) ;
#8849 = ORIENTED_EDGE ( 'NONE', *, *, #19399, .F. ) ;
#8850 = ORIENTED_EDGE ( 'NONE', *, *, #15590, .T. ) ;
#8851 = CARTESIAN_POINT ( 'NONE',  ( -225.9601317720700990, 132.4444111280423613, 15.07876772301852064 ) ) ;
#8852 = CARTESIAN_POINT ( 'NONE',  ( 96.18084660807321029, 232.2996298045118522, 19.72083291508481295 ) ) ;
#8853 = VECTOR ( 'NONE', #7850, 1000.000000000000227 ) ;
#8854 = MANIFOLD_SOLID_BREP ( 'Chamfer2', #22359 ) ;
#8855 = LINE ( 'NONE', #11308, #4357 ) ;
#8856 = FACE_OUTER_BOUND ( 'NONE', #50, .T. ) ;
#8857 = ADVANCED_FACE ( 'NONE', ( #27070 ), #15460, .F. ) ;
#8858 = LINE ( 'NONE', #4260, #8278 ) ;
#8859 = CYLINDRICAL_SURFACE ( 'NONE', #14927, 5.000000000000004441 ) ;
#8860 = FACE_OUTER_BOUND ( 'NONE', #20208, .T. ) ;
#8861 = DIRECTION ( 'NONE',  ( 1.000000000000000000, 0.000000000000000000, -0.000000000000000000 ) ) ;
#8862 = CARTESIAN_POINT ( 'NONE',  ( 139.9999999999994600, -220.0000000000005400, -169.9999999999996874 ) ) ;
#8863 = CARTESIAN_POINT ( 'NONE',  ( 157.4999999999997158, 261.3799376238655441, 45.00000000000000000 ) ) ;
#8864 = CARTESIAN_POINT ( 'NONE',  ( 157.9999999999997158, 256.6181251126050711, 45.00000000000000000 ) ) ;
#8865 = DIRECTION ( 'NONE',  ( 0.8916010070297643031, -0.4528218681374719945, 0.000000000000000000 ) ) ;
#8866 = EDGE_CURVE ( 'NONE', #21473, #14934, #16310, .T. ) ;
#8867 = ORIENTED_EDGE ( 'NONE', *, *, #23113, .T. ) ;
#8868 = AXIS2_PLACEMENT_3D ( 'NONE', #4920, #8812, #17858 ) ;
#8869 = DIRECTION ( 'NONE',  ( 0.8916010070299876800, -0.4528218681370323462, 0.000000000000000000 ) ) ;
#8870 = EDGE_CURVE ( 'NONE', #18977, #3239, #18458, .T. ) ;
#8871 = VECTOR ( 'NONE', #9555, 1000.000000000000000 ) ;
#8872 = CARTESIAN_POINT ( 'NONE',  ( 111.2621361164573131, 140.0000000000000000, 95.03618980370902136 ) ) ;
#8873 = DIRECTION ( 'NONE',  ( 0.4528218681370711485, -0.8916010070299680290, 0.000000000000000000 ) ) ;
#8874 = EDGE_CURVE ( 'NONE', #5833, #26994, #20607, .T. ) ;
#8875 = CARTESIAN_POINT ( 'NONE',  ( 65.00000000000000000, -120.0000000000000711, 70.00000000000001421 ) ) ;
#8876 = VECTOR ( 'NONE', #13910, 1000.000000000000000 ) ;
#8877 = ORIENTED_EDGE ( 'NONE', *, *, #24863, .T. ) ;
#8878 = DIRECTION ( 'NONE',  ( 0.000000000000000000, 0.000000000000000000, -1.000000000000000000 ) ) ;
#8879 = ORIENTED_EDGE ( 'NONE', *, *, #19514, .F. ) ;
#8880 = SURFACE_STYLE_USAGE ( .BOTH. , #26878 ) ;
#8881 = EDGE_LOOP ( 'NONE', ( #14167, #5228, #21092, #21123 ) ) ;
#8882 = ORIENTED_EDGE ( 'NONE', *, *, #26431, .T. ) ;
#8883 = VERTEX_POINT ( 'NONE', #18592 ) ;
#8884 = EDGE_CURVE ( 'NONE', #8985, #19265, #27596, .T. ) ;
#8885 = ORIENTED_EDGE ( 'NONE', *, *, #15432, .F. ) ;
#8886 = CARTESIAN_POINT ( 'NONE',  ( 157.4999999999998579, 168.5885623461056184, -45.00000000000000000 ) ) ;
#8887 = VECTOR ( 'NONE', #26435, 1000.000000000000000 ) ;
#8888 = CARTESIAN_POINT ( 'NONE',  ( -279.1278187736259611, -165.0000000000001421, 106.1966075482099399 ) ) ;
#8889 = VECTOR ( 'NONE', #17711, 1000.000000000000000 ) ;
#8890 = CARTESIAN_POINT ( 'NONE',  ( 157.4999999999998579, 105.8916871584295478, -45.00000000000000000 ) ) ;
#8891 = VECTOR ( 'NONE', #2072, 1000.000000000000000 ) ;
#8892 = UNCERTAINTY_MEASURE_WITH_UNIT (LENGTH_MEASURE( 1.000000000000000082E-05 ), #10431, 'distance_accuracy_value', 'NONE');
#8893 = DIRECTION ( 'NONE',  ( 1.000000000000000000, 0.000000000000000000, 0.000000000000000000 ) ) ;
#8894 = CARTESIAN_POINT ( 'NONE',  ( -214.6111699653978349, 58.62522005596079566, 31.77808924749080788 ) ) ;
#8895 = CARTESIAN_POINT ( 'NONE',  ( 209.9999999999999432, -150.0000000000000284, 99.99999999999991473 ) ) ;
#8896 = DIRECTION ( 'NONE',  ( -1.000000000000000000, 0.000000000000000000, 0.000000000000000000 ) ) ;
#8897 = LINE ( 'NONE', #26693, #22762 ) ;
#8898 = DIRECTION ( 'NONE',  ( -0.000000000000000000, -0.000000000000000000, 1.000000000000000000 ) ) ;
#8899 = CARTESIAN_POINT ( 'NONE',  ( 157.4999999999998579, 128.4625622259929401, -45.00000000000000000 ) ) ;
#8900 = DIRECTION ( 'NONE',  ( 0.8916010070293383105, -0.4528218681383106015, 0.000000000000000000 ) ) ;
#8901 = ADVANCED_FACE ( 'NONE', ( #20325 ), #10192, .T. ) ;
#8902 = ADVANCED_FACE ( 'NONE', ( #9419 ), #20469, .T. ) ;
#8903 = MANIFOLD_SOLID_BREP ( 'Boss-Extrude12', #14105 ) ;
#8904 = DIRECTION ( 'NONE',  ( 1.000000000000000000, 0.000000000000000000, 0.000000000000000000 ) ) ;
#8905 = EDGE_CURVE ( 'NONE', #23195, #15531, #14025, .T. ) ;
#8906 = CARTESIAN_POINT ( 'NONE',  ( 51.56615429303207065, 203.2034914284457159, 15.00000000000000000 ) ) ;
#8907 = LINE ( 'NONE', #2423, #8786 ) ;
#8908 = CARTESIAN_POINT ( 'NONE',  ( 135.9999999999998295, 242.9999999999997158, 45.00000000000000000 ) ) ;
#8910 = EDGE_LOOP ( 'NONE', ( #8670, #21267 ) ) ;
#8909 = ORIENTED_EDGE ( 'NONE', *, *, #27850, .F. ) ;
#8911 = VECTOR ( 'NONE', #15725, 1000.000000000000000 ) ;
#8912 = CARTESIAN_POINT ( 'NONE',  ( -224.1705500038237346, 86.90025305032594360, -16.85721464638110234 ) ) ;
#8913 = CARTESIAN_POINT ( 'NONE',  ( -203.9013263906359441, 92.43596962530546080, -29.05832367954837281 ) ) ;
#8914 = ORIENTED_EDGE ( 'NONE', *, *, #19674, .F. ) ;
#8915 = VECTOR ( 'NONE', #23599, 1000.000000000000000 ) ;
#8916 = VERTEX_POINT ( 'NONE', #5236 ) ;
#8917 = VERTEX_POINT ( 'NONE', #22906 ) ;
#8918 = CARTESIAN_POINT ( 'NONE',  ( -226.9194690495522764, 131.5555540326517985, -13.00000000000000178 ) ) ;
#8919 = CARTESIAN_POINT ( 'NONE',  ( -137.5210505075045262, 129.0054383906156374, 17.05624534316643803 ) ) ;
#8920 = ORIENTED_EDGE ( 'NONE', *, *, #19214, .F. ) ;
#8921 = CARTESIAN_POINT ( 'NONE',  ( 94.38583646783695258, 113.6320904521875548, -75.15625000023771918 ) ) ;
#8922 =( REPRESENTATION_RELATIONSHIP ('NONE','NONE', #11963, #14145 ) REPRESENTATION_RELATIONSHIP_WITH_TRANSFORMATION ( #11363 )SHAPE_REPRESENTATION_RELATIONSHIP( ) );
#8923 = DIRECTION ( 'NONE',  ( 1.000000000000000000, -0.000000000000000000, -0.000000000000000000 ) ) ;
#8924 = VERTEX_POINT ( 'NONE', #7546 ) ;
#8925 = CARTESIAN_POINT ( 'NONE',  ( -216.0630910827463254, 87.83017798286152811, 18.79139027124664096 ) ) ;
#8926 = CIRCLE ( 'NONE', #19018, 5.000000000000004441 ) ;
#8927 = DIRECTION ( 'NONE',  ( 1.000000000000000000, 0.000000000000000000, -0.000000000000000000 ) ) ;
#8928 = LINE ( 'NONE', #17403, #3400 ) ;
#8929 = AXIS2_PLACEMENT_3D ( 'NONE', #27965, #21514, #4127 ) ;
#8930 = CARTESIAN_POINT ( 'NONE',  ( 157.9898533828750260, 200.7262996950787510, -141.9943226514403420 ) ) ;
#8931 = EDGE_CURVE ( 'NONE', #1390, #14300, #24639, .T. ) ;
#8932 = ORIENTED_EDGE ( 'NONE', *, *, #23776, .F. ) ;
#8933 = DIRECTION ( 'NONE',  ( 0.000000000000000000, 0.000000000000000000, -1.000000000000000000 ) ) ;
#8934 = EDGE_CURVE ( 'NONE', #23123, #8669, #119, .T. ) ;
#8935 = CARTESIAN_POINT ( 'NONE',  ( 157.4999999999997442, 251.3484375938375024, -45.00000000000000000 ) ) ;
#8936 = DIRECTION ( 'NONE',  ( 0.8916010070293995948, 0.4528218681381900312, 0.000000000000000000 ) ) ;
#8937 = DIRECTION ( 'NONE',  ( -0.8314772792026879911, 0.5555587585212703461, 0.000000000000000000 ) ) ;
#8938 = ORIENTED_EDGE ( 'NONE', *, *, #27083, .T. ) ;
#8939 = DIRECTION ( 'NONE',  ( -1.000000000000000000, 5.551115123125784674E-16, 0.000000000000000000 ) ) ;
#8940 = DIRECTION ( 'NONE',  ( -0.05364526231778202897, 0.9985600561963492439, 0.000000000000000000 ) ) ;
#8941 = CARTESIAN_POINT ( 'NONE',  ( -143.0445616319559008, 68.96623314385857384, 82.96749942560525426 ) ) ;
#8942 = ORIENTED_EDGE ( 'NONE', *, *, #25848, .F. ) ;
#8943 =( LENGTH_UNIT ( ) NAMED_UNIT ( * ) SI_UNIT ( .MILLI., .METRE. ) );
#8944 = AXIS2_PLACEMENT_3D ( 'NONE', #24511, #1955, #13318 ) ;
#8945 = EDGE_LOOP ( 'NONE', ( #9879, #2319, #24213, #15036, #10800 ) ) ;
#8946 = VECTOR ( 'NONE', #18677, 1000.000000000000000 ) ;
#8947 = DIRECTION ( 'NONE',  ( 0.8916010070294598799, -0.4528218681380714594, 0.000000000000000000 ) ) ;
#8948 = CARTESIAN_POINT ( 'NONE',  ( -185.5061758263113632, 106.4823051942665302, -31.41754718802355839 ) ) ;
#8949 = VERTEX_POINT ( 'NONE', #12566 ) ;
#8950 = CIRCLE ( 'NONE', #25010, 2.586968381275096984 ) ;
#8951 = EDGE_LOOP ( 'NONE', ( #21174, #4801, #23229, #27831 ) ) ;
#8952 = CARTESIAN_POINT ( 'NONE',  ( 157.9999999999997158, 259.1260001201120531, -45.00000000000000000 ) ) ;
#8953 = CARTESIAN_POINT ( 'NONE',  ( 217.4999999999996305, -5.589247009368160768, 100.0000000000000142 ) ) ;
#8954 = ORIENTED_EDGE ( 'NONE', *, *, #12561, .T. ) ;
#8955 = ORIENTED_EDGE ( 'NONE', *, *, #16972, .T. ) ;
#8956 = CARTESIAN_POINT ( 'NONE',  ( -0.4700637257060664709, 134.1129467060154070, 15.56863088294750064 ) ) ;
#8957 = EDGE_CURVE ( 'NONE', #4617, #17073, #27620, .T. ) ;
#8958 = CYLINDRICAL_SURFACE ( 'NONE', #19525, 41.00000000000000711 ) ;
#8959 = CIRCLE ( 'NONE', #8513, 34.99999999999997868 ) ;
#8960 = LINE ( 'NONE', #17719, #20837 ) ;
#8961 = DIRECTION ( 'NONE',  ( 0.000000000000000000, -0.9612513907525602752, -0.2756732917354685064 ) ) ;
#8962 = CARTESIAN_POINT ( 'NONE',  ( 157.4999999999998579, 108.3995621659365867, 45.00000000000000000 ) ) ;
#8963 = AXIS2_PLACEMENT_3D ( 'NONE', #4264, #2104, #10883 ) ;
#8964 = CARTESIAN_POINT ( 'NONE',  ( -209.4684130045736197, 67.32370550333207859, -34.40586572994357084 ) ) ;
#8965 = DIRECTION ( 'NONE',  ( 0.000000000000000000, 1.000000000000000000, 0.000000000000000000 ) ) ;
#8966 = VERTEX_POINT ( 'NONE', #5800 ) ;
#8967 = FACE_OUTER_BOUND ( 'NONE', #5097, .T. ) ;
#8968 = ADVANCED_FACE ( 'NONE', ( #1759 ), #1626, .F. ) ;
#8969 = AXIS2_PLACEMENT_3D ( 'NONE', #10785, #23571, #1860 ) ;
#8970 = DIRECTION ( 'NONE',  ( 0.8916010070299064116, -0.4528218681371922183, 0.000000000000000000 ) ) ;
#8971 = DIRECTION ( 'NONE',  ( 0.000000000000000000, 0.000000000000000000, -1.000000000000000000 ) ) ;
#8972 = CARTESIAN_POINT ( 'NONE',  ( 157.9999999999998010, 239.0630000600560550, 45.00000000000000000 ) ) ;
#8973 = ORIENTED_EDGE ( 'NONE', *, *, #4077, .F. ) ;
#8974 = CARTESIAN_POINT ( 'NONE',  ( -215.0412094859541980, 60.20193349634168101, 13.76727271988285040 ) ) ;
#8975 = ORIENTED_EDGE ( 'NONE', *, *, #16527, .F. ) ;
#8976 = EDGE_CURVE ( 'NONE', #2948, #27477, #22139, .T. ) ;
#8977 = CARTESIAN_POINT ( 'NONE',  ( 142.6536686473019699, 201.5224093497741649, 45.00000000000000000 ) ) ;
#8978 = DIRECTION ( 'NONE',  ( 1.000000000000000000, -0.000000000000000000, -0.000000000000000000 ) ) ;
#8979 = LINE ( 'NONE', #4511, #18593 ) ;
#8980 = ORIENTED_EDGE ( 'NONE', *, *, #20287, .F. ) ;
#8981 = CARTESIAN_POINT ( 'NONE',  ( 158.0000000000003979, 168.8424998498591663, 45.00000000000000000 ) ) ;
#8982 = FILL_AREA_STYLE ('',( #6397 ) ) ;
#8983 = VERTEX_POINT ( 'NONE', #16585 ) ;
#8984 = DIRECTION ( 'NONE',  ( 1.000000000000000000, -0.000000000000000000, -0.000000000000000000 ) ) ;
#8985 = VERTEX_POINT ( 'NONE', #5661 ) ;
#8986 = DIRECTION ( 'NONE',  ( 1.000000000000000000, 0.000000000000000000, -0.000000000000000000 ) ) ;
#8987 = ORIENTED_EDGE ( 'NONE', *, *, #13845, .F. ) ;
#8988 = AXIS2_PLACEMENT_3D ( 'NONE', #20868, #5639, #1465 ) ;
#8989 = AXIS2_PLACEMENT_3D ( 'NONE', #7702, #18201, #11606 ) ;
#8990 = CIRCLE ( 'NONE', #24125, 6.025000000000002132 ) ;
#8991 = EDGE_CURVE ( 'NONE', #3649, #28003, #1487, .T. ) ;
#8992 = EDGE_LOOP ( 'NONE', ( #18499, #4453, #3741, #5104 ) ) ;
#8993 = CARTESIAN_POINT ( 'NONE',  ( 179.9999999999999147, 494.4107529906318632, -100.0000000000000142 ) ) ;
#8994 = ORIENTED_EDGE ( 'NONE', *, *, #2234, .F. ) ;
#8995 = CIRCLE ( 'NONE', #14061, 6.000000000000005329 ) ;
#8996 = ORIENTED_EDGE ( 'NONE', *, *, #9459, .T. ) ;
#8997 = CARTESIAN_POINT ( 'NONE',  ( -220.9676528974450491, 136.4492860810096317, 15.12837422688856925 ) ) ;
#8998 = CARTESIAN_POINT ( 'NONE',  ( 102.0190107526936174, 244.0003474240143078, 16.44012727447546496 ) ) ;
#8999 = EDGE_CURVE ( 'NONE', #14199, #17744, #25339, .T. ) ;
#9000 = DIRECTION ( 'NONE',  ( 0.000000000000000000, 0.000000000000000000, 1.000000000000000000 ) ) ;
#9001 = DIRECTION ( 'NONE',  ( -0.000000000000000000, 1.000000000000000000, -1.387778780781445429E-16 ) ) ;
#9002 = DIRECTION ( 'NONE',  ( 1.000000000000000000, 0.000000000000000000, -0.000000000000000000 ) ) ;
#9003 = CARTESIAN_POINT ( 'NONE',  ( -277.2150368962633706, -170.0000000000001137, 90.47363622314041720 ) ) ;
#9004 = DIRECTION ( 'NONE',  ( 0.000000000000000000, 0.000000000000000000, -1.000000000000000000 ) ) ;
#9005 = CARTESIAN_POINT ( 'NONE',  ( 232.4999999999996305, 133.0668745871126930, -42.88984227207694744 ) ) ;
#9006 = LINE ( 'NONE', #21798, #17224 ) ;
#9007 = CARTESIAN_POINT ( 'NONE',  ( -230.8916957670046486, 130.8330661503599117, -15.00000000000000000 ) ) ;
#9008 = LINE ( 'NONE', #20492, #22414 ) ;
#9009 = DIRECTION ( 'NONE',  ( -0.2066290158914688702, -0.9784193629480781862, 0.000000000000000000 ) ) ;
#9010 = VECTOR ( 'NONE', #15, 1000.000000000000000 ) ;
#9011 = VERTEX_POINT ( 'NONE', #14571 ) ;
#9012 = PLANE ( 'NONE',  #18834 ) ;
#9013 = ADVANCED_FACE ( 'NONE', ( #23607 ), #3778, .F. ) ;
#9014 = EDGE_CURVE ( 'NONE', #3225, #19223, #6534, .T. ) ;
#9015 = DIRECTION ( 'NONE',  ( 1.000000000000000000, 0.000000000000000000, 0.000000000000000000 ) ) ;
#9016 = DIRECTION ( 'NONE',  ( -2.602085213965210642E-16, 1.000000000000000000, 0.000000000000000000 ) ) ;
#9017 = CARTESIAN_POINT ( 'NONE',  ( -225.7036482868739427, -91.18033988749901653, -18.91107291867258411 ) ) ;
#9018 =( BOUNDED_SURFACE ( )  B_SPLINE_SURFACE ( 3, 2, ( 
 ( #10073, #23420, #14389 ),
 ( #3730, #21406, #1720 ),
 ( #23147, #19253, #23001 ),
 ( #8340, #8192, #18825 ),
 ( #12243, #27573, #25435 ),
 ( #25150, #12520, #12103 ),
 ( #16681, #27715, #21264 ),
 ( #5755, #14529, #16822 ),
 ( #25997, #10638, #28143 ),
 ( #12945, #11065, #23709 ),
 ( #17666, #10921, #19394 ),
 ( #21696, #2286, #13370 ),
 ( #8483, #10784, #11210 ),
 ( #17520, #15245, #6744 ),
 ( #21548, #17237, #6180 ),
 ( #25855, #19819, #4159 ),
 ( #2007, #4584, #23998 ),
 ( #26419, #19682, #19542 ),
 ( #4309, #6, #6315 ),
 ( #14956, #24143, #2148 ),
 ( #19964, #12802, #21842 ),
 ( #13094, #8765, #22121 ) ),
 .UNSPECIFIED., .F., .F., .F. ) 
 B_SPLINE_SURFACE_WITH_KNOTS ( ( 4, 2, 2, 2, 2, 2, 2, 2, 2, 2, 4 ),
 ( 3, 3 ),
 ( 0.000000000000000000, 0.006464363597911549145, 0.01292872719582309829, 0.01616090899477887199, 0.01939309079373464917, 0.02585745439164619658, 0.02908963619060197028, 0.03232181798955774399, 0.03878618158746929834, 0.04525054518538084575, 0.05171490878329239316 ),
 ( 0.000000000000000000, 1.000000000000000000 ),
 .UNSPECIFIED. ) 
 GEOMETRIC_REPRESENTATION_ITEM ( )  RATIONAL_B_SPLINE_SURFACE ( (
 ( 1.000000000000000000, 0.9597817246759321463, 1.000000000000000000),
 ( 1.000000000000000000, 0.9644978604548086754, 1.000000000000000000),
 ( 1.000000000000000000, 0.9684366129255929101, 1.000000000000000000),
 ( 1.000000000000000000, 0.9744801429909556445, 1.000000000000000000),
 ( 1.000000000000000000, 0.9765856948512464664, 1.000000000000000000),
 ( 1.000000000000000000, 0.9781316547679167472, 1.000000000000000000),
 ( 1.000000000000000000, 0.9783777913778298752, 1.000000000000000000),
 ( 1.000000000000000000, 0.9782912468864014555, 1.000000000000000000),
 ( 1.000000000000000000, 0.9779594306925435410, 1.000000000000000000),
 ( 1.000000000000000000, 0.9761609493688950812, 1.000000000000000000),
 ( 1.000000000000000000, 0.9738931452053198878, 1.000000000000000000),
 ( 1.000000000000000000, 0.9691275407867268044, 1.000000000000000000),
 ( 1.000000000000000000, 0.9673113114069962215, 1.000000000000000000),
 ( 1.000000000000000000, 0.9632590755101273494, 1.000000000000000000),
 ( 1.000000000000000000, 0.9610203127353997843, 1.000000000000000000),
 ( 1.000000000000000000, 0.9537484340619055700, 1.000000000000000000),
 ( 1.000000000000000000, 0.9481631559643158846, 1.000000000000000000),
 ( 1.000000000000000000, 0.9357596895728105268, 1.000000000000000000),
 ( 1.000000000000000000, 0.9289410327529883382, 1.000000000000000000),
 ( 1.000000000000000000, 0.9142674582240357672, 1.000000000000000000),
 ( 1.000000000000000000, 0.9064119848472056429, 1.000000000000000000),
 ( 1.000000000000000000, 0.8981184559478653240, 1.000000000000000000) ) ) 
 REPRESENTATION_ITEM ( '' )  SURFACE ( )  );
#9019 = VECTOR ( 'NONE', #26060, 1000.000000000000000 ) ;
#9020 = VERTEX_POINT ( 'NONE', #14997 ) ;
#9021 = CARTESIAN_POINT ( 'NONE',  ( 109.9999999999998863, 260.0000000000000000, -45.00000000000000000 ) ) ;
#9022 = VERTEX_POINT ( 'NONE', #23325 ) ;
#9023 = DIRECTION ( 'NONE',  ( 0.000000000000000000, 0.000000000000000000, 1.000000000000000000 ) ) ;
#9024 = ORIENTED_EDGE ( 'NONE', *, *, #20567, .F. ) ;
#9025 = EDGE_CURVE ( 'NONE', #13229, #15076, #4699, .T. ) ;
#9026 = ORIENTED_EDGE ( 'NONE', *, *, #12017, .T. ) ;
#9027 = ORIENTED_EDGE ( 'NONE', *, *, #19877, .F. ) ;
#9028 = ORIENTED_EDGE ( 'NONE', *, *, #17194, .F. ) ;
#9029 = ORIENTED_EDGE ( 'NONE', *, *, #13426, .T. ) ;
#9030 = LINE ( 'NONE', #8886, #2618 ) ;
#9031 = VECTOR ( 'NONE', #6931, 1000.000000000000000 ) ;
#9032 = LINE ( 'NONE', #13640, #20532 ) ;
#9033 = CARTESIAN_POINT ( 'NONE',  ( 134.9999999999998579, 404.6636166603179277, -145.0000000000000000 ) ) ;
#9034 = EDGE_CURVE ( 'NONE', #4647, #20791, #17141, .T. ) ;
#9035 = DIRECTION ( 'NONE',  ( -1.000000000000000000, -0.000000000000000000, -0.000000000000000000 ) ) ;
#9036 = ADVANCED_FACE ( 'NONE', ( #28036 ), #27896, .F. ) ;
#9037 = CARTESIAN_POINT ( 'NONE',  ( 158.0000000000004263, 168.3346248423521274, -45.00000000000000000 ) ) ;
#9038 = CARTESIAN_POINT ( 'NONE',  ( -212.5256769160629631, 72.66764018259519275, 29.94823517519424527 ) ) ;
#9039 = FACE_OUTER_BOUND ( 'NONE', #20536, .T. ) ;
#9040 = DIRECTION ( 'NONE',  ( 0.000000000000000000, -1.214306433183764966E-16, 1.000000000000000000 ) ) ;
#9041 = LINE ( 'NONE', #6597, #10366 ) ;
#9042 = DIRECTION ( 'NONE',  ( 0.8916010070298353574, -0.4528218681373320509, 0.000000000000000000 ) ) ;
#9043 = LINE ( 'NONE', #10627, #20088 ) ;
#9044 = DIRECTION ( 'NONE',  ( 0.000000000000000000, -1.000000000000000000, 0.000000000000000000 ) ) ;
#9045 = CARTESIAN_POINT ( 'NONE',  ( 4.492022713026529779, 138.9219254684496718, 13.09535121465864727 ) ) ;
#9046 = DIRECTION ( 'NONE',  ( -0.000000000000000000, -1.000000000000000000, -0.000000000000000000 ) ) ;
#9047 = CARTESIAN_POINT ( 'NONE',  ( -167.6265986190112187, 116.3518912474305296, 25.91344288888009473 ) ) ;
#9048 = CARTESIAN_POINT ( 'NONE',  ( -68.97958094182604327, 102.2323340340523288, -127.0692718809191035 ) ) ;
#9050 = VERTEX_POINT ( 'NONE', #10397 ) ;
#9049 = EDGE_LOOP ( 'NONE', ( #5045, #9127, #21873, #10647 ) ) ;
#9051 = VECTOR ( 'NONE', #20005, 1000.000000000000000 ) ;
#9052 = CARTESIAN_POINT ( 'NONE',  ( 187.4999999999996305, -5.589247009368136787, -100.0000000000000142 ) ) ;
#9053 = CARTESIAN_POINT ( 'NONE',  ( 0.000000000000000000, 0.000000000000000000, -45.00000000000000000 ) ) ;
#9054 = CARTESIAN_POINT ( 'NONE',  ( -205.5650550490929902, 90.70191985663102230, -28.50364138414912318 ) ) ;
#9055 = EDGE_LOOP ( 'NONE', ( #19863, #13100, #8126, #335 ) ) ;
#9056 = ORIENTED_EDGE ( 'NONE', *, *, #24444, .F. ) ;
#9057 = ORIENTED_EDGE ( 'NONE', *, *, #17061, .F. ) ;
#9058 = CARTESIAN_POINT ( 'NONE',  ( 187.4999999999996305, 83.06687458711267880, -36.86484227207694175 ) ) ;
#9059 = CARTESIAN_POINT ( 'NONE',  ( -137.1120637285174269, 127.8502071294020368, 17.56806758514733247 ) ) ;
#9060 = ORIENTED_EDGE ( 'NONE', *, *, #10081, .T. ) ;
#9061 = EDGE_CURVE ( 'NONE', #1176, #12421, #27480, .T. ) ;
#9062 = VERTEX_POINT ( 'NONE', #25749 ) ;
#9063 = PLANE ( 'NONE',  #4912 ) ;
#9064 = ADVANCED_FACE ( 'NONE', ( #6079 ), #14861, .T. ) ;
#9065 = CARTESIAN_POINT ( 'NONE',  ( 157.4999999999998010, 233.7933125412885147, -45.00000000000000000 ) ) ;
#9066 = VERTEX_POINT ( 'NONE', #14434 ) ;
#9067 = LINE ( 'NONE', #7055, #3634 ) ;
#9068 = VECTOR ( 'NONE', #2129, 1000.000000000000000 ) ;
#9069 = DIRECTION ( 'NONE',  ( -0.000000000000000000, -0.000000000000000000, -1.000000000000000000 ) ) ;
#9070 = AXIS2_PLACEMENT_3D ( 'NONE', #17466, #21638, #16141 ) ;
#9071 = CARTESIAN_POINT ( 'NONE',  ( 179.9999999999999147, 494.4107529906318632, 84.99999999999997158 ) ) ;
#9072 = CARTESIAN_POINT ( 'NONE',  ( 160.4757310268322499, 204.1562516397053173, -139.0778438077165902 ) ) ;
#9073 = CARTESIAN_POINT ( 'NONE',  ( -214.0383293111087539, 72.11341309493322171, -27.85175881924293506 ) ) ;
#9074 = ORIENTED_EDGE ( 'NONE', *, *, #17460, .F. ) ;
#9075 = DIRECTION ( 'NONE',  ( 0.000000000000000000, 0.000000000000000000, -1.000000000000000000 ) ) ;
#9076 = CARTESIAN_POINT ( 'NONE',  ( -225.9729034214342391, 132.4331356209129922, -12.99353264123096885 ) ) ;
#9077 = CARTESIAN_POINT ( 'NONE',  ( -180.0000000000000284, -40.00000000000004974, 70.00000000000000000 ) ) ;
#9078 = DIRECTION ( 'NONE',  ( -0.8916010070297345491, -0.4528218681375307253, 0.000000000000000000 ) ) ;
#9079 = EDGE_LOOP ( 'NONE', ( #28396, #16623, #4703, #7408 ) ) ;
#9080 = LINE ( 'NONE', #24172, #874 ) ;
#9081 = AXIS2_PLACEMENT_3D ( 'NONE', #12062, #23110, #21368 ) ;
#9082 = ADVANCED_FACE ( 'NONE', ( #10537 ), #8381, .F. ) ;
#9083 = CARTESIAN_POINT ( 'NONE',  ( 157.4999999999998579, 50.71843699327460797, 45.00000000000000000 ) ) ;
#9084 = AXIS2_PLACEMENT_3D ( 'NONE', #5079, #22619, #27197 ) ;
#9085 = CARTESIAN_POINT ( 'NONE',  ( -142.3242417476000981, 69.93676590415873306, 82.90331240453681971 ) ) ;
#9086 = ORIENTED_EDGE ( 'NONE', *, *, #24082, .F. ) ;
#9087 = ORIENTED_EDGE ( 'NONE', *, *, #5464, .T. ) ;
#9088 = LINE ( 'NONE', #19581, #23492 ) ;
#9089 = CARTESIAN_POINT ( 'NONE',  ( -199.9534950421034125, 95.77273280906791797, -30.16924513461026081 ) ) ;
#9090 = ORIENTED_EDGE ( 'NONE', *, *, #26653, .T. ) ;
#9091 = EDGE_CURVE ( 'NONE', #12262, #6349, #18870, .T. ) ;
#9092 = ORIENTED_EDGE ( 'NONE', *, *, #9758, .T. ) ;
#9093 = EDGE_CURVE ( 'NONE', #4814, #17928, #24852, .T. ) ;
#9094 = CARTESIAN_POINT ( 'NONE',  ( 157.9999999999998579, 221.0000000000000284, 45.00000000000000000 ) ) ;
#9095 = EDGE_CURVE ( 'NONE', #12922, #16796, #4199, .T. ) ;
#9096 = LINE ( 'NONE', #8673, #7526 ) ;
#9097 = MECHANICAL_DESIGN_GEOMETRIC_PRESENTATION_REPRESENTATION (  '', ( #19179 ), #4037 ) ;
#9098 = ADVANCED_FACE ( 'NONE', ( #13808 ), #22556, .F. ) ;
#9099 = ORIENTED_EDGE ( 'NONE', *, *, #17499, .T. ) ;
#9100 = ORIENTED_EDGE ( 'NONE', *, *, #8077, .F. ) ;
#9101 = LINE ( 'NONE', #22026, #10694 ) ;
#9102 = AXIS2_PLACEMENT_3D ( 'NONE', #16912, #13570, #11119 ) ;
#9103 = CARTESIAN_POINT ( 'NONE',  ( 157.4999999999998579, 181.1279373836408411, 45.00000000000000000 ) ) ;
#9104 = LINE ( 'NONE', #26614, #21743 ) ;
#9105 = CARTESIAN_POINT ( 'NONE',  ( -27.08985507592738173, 129.1630599246555562, -15.68767261356309284 ) ) ;
#9106 = LINE ( 'NONE', #17864, #12787 ) ;
#9107 = DIRECTION ( 'NONE',  ( -1.000000000000000000, -8.673617379884036705E-17, -0.000000000000000000 ) ) ;
#9108 = CARTESIAN_POINT ( 'NONE',  ( -180.0000000000000284, -50.00000000000004263, 110.0000000000000284 ) ) ;
#9109 = ORIENTED_EDGE ( 'NONE', *, *, #22755, .F. ) ;
#9110 = FACE_OUTER_BOUND ( 'NONE', #18733, .T. ) ;
#9111 = CARTESIAN_POINT ( 'NONE',  ( 157.9999999999998579, 223.5078750075070104, -45.00000000000000000 ) ) ;
#9112 = DIRECTION ( 'NONE',  ( -0.000000000000000000, -0.000000000000000000, -1.000000000000000000 ) ) ;
#9113 = CARTESIAN_POINT ( 'NONE',  ( 157.4999999999995737, 203.6988124512014338, 45.00000000000000000 ) ) ;
#9114 = VERTEX_POINT ( 'NONE', #6891 ) ;
#9115 = DIRECTION ( 'NONE',  ( -0.000000000000000000, 0.000000000000000000, -1.000000000000000000 ) ) ;
#9116 = VERTEX_POINT ( 'NONE', #28181 ) ;
#9117 = AXIS2_PLACEMENT_3D ( 'NONE', #25926, #6249, #3524 ) ;
#9118 = LINE ( 'NONE', #26208, #3817 ) ;
#9119 = DIRECTION ( 'NONE',  ( 0.000000000000000000, 0.000000000000000000, 1.000000000000000000 ) ) ;
#9120 = CARTESIAN_POINT ( 'NONE',  ( 140.7972055090965853, 249.4346022597576393, -146.5591841905931290 ) ) ;
#9121 = ORIENTED_EDGE ( 'NONE', *, *, #2322, .F. ) ;
#9122 = FACE_OUTER_BOUND ( 'NONE', #4666, .T. ) ;
#9123 = ORIENTED_EDGE ( 'NONE', *, *, #549, .T. ) ;
#9124 = CIRCLE ( 'NONE', #19683, 22.49999999999999289 ) ;
#9125 = EDGE_CURVE ( 'NONE', #14251, #11388, #22267, .T. ) ;
#9126 = DIRECTION ( 'NONE',  ( -0.000000000000000000, -0.000000000000000000, -1.000000000000000000 ) ) ;
#9127 = ORIENTED_EDGE ( 'NONE', *, *, #6544, .T. ) ;
#9128 = CARTESIAN_POINT ( 'NONE',  ( 367.4999999999996021, 44.41075299063185611, -75.00000000000001421 ) ) ;
#9129 = ADVANCED_FACE ( 'NONE', ( #20250 ), #2430, .F. ) ;
#9130 = AXIS2_PLACEMENT_3D ( 'NONE', #16566, #23170, #5780 ) ;
#9131 = ORIENTED_EDGE ( 'NONE', *, *, #11305, .F. ) ;
#9132 = ORIENTED_EDGE ( 'NONE', *, *, #2105, .T. ) ;
#9133 = CIRCLE ( 'NONE', #14188, 53.86582179324592090 ) ;
#9134 = LINE ( 'NONE', #8846, #17714 ) ;
#9135 = ORIENTED_EDGE ( 'NONE', *, *, #8387, .T. ) ;
#9136 = EDGE_CURVE ( 'NONE', #7154, #24450, #22600, .T. ) ;
#9137 = ORIENTED_EDGE ( 'NONE', *, *, #3666, .F. ) ;
#9138 = ORIENTED_EDGE ( 'NONE', *, *, #22171, .T. ) ;
#9139 = CARTESIAN_POINT ( 'NONE',  ( 98.16608178754300695, 241.2913188899314036, 20.91842009985186124 ) ) ;
#9140 = EDGE_CURVE ( 'NONE', #9424, #21412, #23893, .T. ) ;
#9141 = VECTOR ( 'NONE', #20315, 999.9999999999998863 ) ;
#9142 = DIRECTION ( 'NONE',  ( 0.000000000000000000, 0.000000000000000000, -1.000000000000000000 ) ) ;
#9143 = AXIS2_PLACEMENT_3D ( 'NONE', #1395, #18921, #18366 ) ;
#9144 = LINE ( 'NONE', #4530, #2749 ) ;
#9145 = DIRECTION ( 'NONE',  ( 1.000000000000000000, 0.000000000000000000, 0.000000000000000000 ) ) ;
#9146 = VECTOR ( 'NONE', #2859, 1000.000000000000000 ) ;
#9147 = DIRECTION ( 'NONE',  ( 0.000000000000000000, 1.000000000000000000, 0.000000000000000000 ) ) ;
#9148 = CARTESIAN_POINT ( 'NONE',  ( 134.9999999999998579, 220.0000000000000284, -105.0000000000000284 ) ) ;
#9149 = DIRECTION ( 'NONE',  ( 0.000000000000000000, -1.000000000000000000, 0.000000000000000000 ) ) ;
#9150 = CYLINDRICAL_SURFACE ( 'NONE', #8495, 10.00000000000000888 ) ;
#9151 = FACE_OUTER_BOUND ( 'NONE', #16856, .T. ) ;
#9152 = DIRECTION ( 'NONE',  ( -0.000000000000000000, 1.000000000000000000, -1.387778780781445429E-16 ) ) ;
#9153 = DIRECTION ( 'NONE',  ( -0.000000000000000000, 0.000000000000000000, 1.000000000000000000 ) ) ;
#9154 = VECTOR ( 'NONE', #24330, 1000.000000000000114 ) ;
#9155 = EDGE_LOOP ( 'NONE', ( #22309, #9317, #17220, #1912 ) ) ;
#9156 = CARTESIAN_POINT ( 'NONE',  ( 158.0000000000007105, 138.2401247522676044, 45.00000000000000000 ) ) ;
#9157 = VECTOR ( 'NONE', #13969, 1000.000000000000000 ) ;
#9158 = CARTESIAN_POINT ( 'NONE',  ( 157.9999999999998010, 236.0472500450420341, -45.00000000000000000 ) ) ;
#9159 = CARTESIAN_POINT ( 'NONE',  ( 158.0000000000004547, 163.8267498348450886, 45.00000000000000000 ) ) ;
#9160 = CARTESIAN_POINT ( 'NONE',  ( -6.124983682450844166E-17, 0.000000000000000000, 0.000000000000000000 ) ) ;
#9161 = VERTEX_POINT ( 'NONE', #439 ) ;
#9162 = ADVANCED_FACE ( 'NONE', ( #5018 ), #24710, .T. ) ;
#9163 = VECTOR ( 'NONE', #27855, 1000.000000000000000 ) ;
#9164 = DIRECTION ( 'NONE',  ( -0.8660254037844362651, 0.5000000000000039968, -0.000000000000000000 ) ) ;
#9165 = ORIENTED_EDGE ( 'NONE', *, *, #18979, .T. ) ;
#9166 = CARTESIAN_POINT ( 'NONE',  ( -51.90955279280624524, 193.7290884209386661, -45.00000000000000000 ) ) ;
#9167 = VERTEX_POINT ( 'NONE', #15138 ) ;
#9168 = ORIENTED_EDGE ( 'NONE', *, *, #11735, .F. ) ;
#9169 = ORIENTED_EDGE ( 'NONE', *, *, #27631, .F. ) ;
#9170 = ORIENTED_EDGE ( 'NONE', *, *, #9262, .T. ) ;
#9171 = ORIENTED_EDGE ( 'NONE', *, *, #2105, .F. ) ;
#9172 = VERTEX_POINT ( 'NONE', #9199 ) ;
#9173 = PLANE ( 'NONE',  #14122 ) ;
#9174 = CARTESIAN_POINT ( 'NONE',  ( 157.4751130497509450, 224.9869122110685566, -45.00000000000000000 ) ) ;
#9175 = CIRCLE ( 'NONE', #16960, 10.70611877156249214 ) ;
#9176 = ADVANCED_FACE ( 'NONE', ( #2575 ), #1037, .T. ) ;
#9177 = EDGE_CURVE ( 'NONE', #27627, #21518, #1932, .T. ) ;
#9178 = DIRECTION ( 'NONE',  ( -1.530283246943720875E-16, 1.000000000000000000, -0.000000000000000000 ) ) ;
#9179 = LINE ( 'NONE', #22535, #190 ) ;
#9180 = CARTESIAN_POINT ( 'NONE',  ( -220.6363270246480965, 61.10744949787188318, 10.70339401868985796 ) ) ;
#9181 = CARTESIAN_POINT ( 'NONE',  ( -107.3221550338875687, 22.24192588826928585, 80.00000000000001421 ) ) ;
#9182 = CARTESIAN_POINT ( 'NONE',  ( -187.8924994060663494, 156.4650759647683742, -13.00000000000000000 ) ) ;
#9183 = VECTOR ( 'NONE', #24514, 1000.000000000000000 ) ;
#9184 = DIRECTION ( 'NONE',  ( -0.8916010070299273949, -0.4528218681371510845, 0.000000000000000000 ) ) ;
#9185 = DIRECTION ( 'NONE',  ( -0.6681556583950127859, -0.7440215159219033536, 0.000000000000000000 ) ) ;
#9186 = LINE ( 'NONE', #14981, #12903 ) ;
#9187 = DIRECTION ( 'NONE',  ( -0.8916010070297643031, 0.4528218681374719390, 0.000000000000000000 ) ) ;
#9188 = PLANE ( 'NONE',  #1059 ) ;
#9189 = EDGE_CURVE ( 'NONE', #20219, #8776, #18106, .T. ) ;
#9190 = VECTOR ( 'NONE', #3915, 1000.000000000000000 ) ;
#9191 = EDGE_CURVE ( 'NONE', #5762, #1390, #23516, .T. ) ;
#9192 = CARTESIAN_POINT ( 'NONE',  ( -7.763489797328277930, 131.2264966167943498, 16.31092294497945971 ) ) ;
#9193 = LINE ( 'NONE', #26701, #438 ) ;
#9194 = CARTESIAN_POINT ( 'NONE',  ( 157.9999999999998010, 233.5393750375350237, 45.00000000000000000 ) ) ;
#9195 = FACE_OUTER_BOUND ( 'NONE', #6583, .T. ) ;
#9197 = ORIENTED_EDGE ( 'NONE', *, *, #1365, .F. ) ;
#9196 = ORIENTED_EDGE ( 'NONE', *, *, #14878, .T. ) ;
#9198 = CARTESIAN_POINT ( 'NONE',  ( -212.2922668275968192, 87.25497565882355389, -23.57411103248302453 ) ) ;
#9199 = CARTESIAN_POINT ( 'NONE',  ( 112.5248869502488134, 224.9869122110685282, 45.00000000000000000 ) ) ;
#9200 = DIRECTION ( 'NONE',  ( -0.8916010070293383105, -0.4528218681383106015, 0.000000000000000000 ) ) ;
#9201 = VERTEX_POINT ( 'NONE', #17956 ) ;
#9202 = ORIENTED_EDGE ( 'NONE', *, *, #16273, .F. ) ;
#9203 = EDGE_LOOP ( 'NONE', ( #15426, #22675 ) ) ;
#9204 = CARTESIAN_POINT ( 'NONE',  ( 139.9999999999999147, 4.857225732735056078E-14, 70.00000000000001421 ) ) ;
#9205 = AXIS2_PLACEMENT_3D ( 'NONE', #4493, #6800, #17437 ) ;
#9206 = CARTESIAN_POINT ( 'NONE',  ( -160.0000000000000284, 119.7660240611718763, 22.85081902853006142 ) ) ;
#9207 = ORIENTED_EDGE ( 'NONE', *, *, #20903, .F. ) ;
#9208 = VERTEX_POINT ( 'NONE', #7039 ) ;
#9209 = DIRECTION ( 'NONE',  ( -0.000000000000000000, -0.000000000000000000, -1.000000000000000000 ) ) ;
#9210 = AXIS2_PLACEMENT_3D ( 'NONE', #27467, #3622, #5788 ) ;
#9211 = EDGE_CURVE ( 'NONE', #7931, #17036, #5167, .T. ) ;
#9212 = CARTESIAN_POINT ( 'NONE',  ( 158.0000000000016769, 45.95662448201407102, -45.00000000000000000 ) ) ;
#9213 = ORIENTED_EDGE ( 'NONE', *, *, #24150, .F. ) ;
#9214 = CARTESIAN_POINT ( 'NONE',  ( 157.9999999999998579, 0.000000000000000000, -45.00000000000000000 ) ) ;
#9215 = LINE ( 'NONE', #15687, #7524 ) ;
#9216 = CARTESIAN_POINT ( 'NONE',  ( 157.4999999999998579, 73.28931206083800021, -45.00000000000000000 ) ) ;
#9217 = CARTESIAN_POINT ( 'NONE',  ( 158.0000000000016485, 50.46449948952111697, 45.00000000000000000 ) ) ;
#9218 = CARTESIAN_POINT ( 'NONE',  ( -200.3909388570902763, 61.22025098964611090, -27.25552298266465456 ) ) ;
#9219 = ORIENTED_EDGE ( 'NONE', *, *, #19756, .T. ) ;
#9220 = DIRECTION ( 'NONE',  ( 0.000000000000000000, -1.000000000000000000, 0.000000000000000000 ) ) ;
#9221 = CARTESIAN_POINT ( 'NONE',  ( -190.0000000000000284, 59.99999999999995026, 80.00000000000001421 ) ) ;
#9222 = DIRECTION ( 'NONE',  ( 0.000000000000000000, 0.000000000000000000, 1.000000000000000000 ) ) ;
#9223 = PLANE ( 'NONE',  #11218 ) ;
#9224 = VERTEX_POINT ( 'NONE', #24566 ) ;
#9225 = EDGE_CURVE ( 'NONE', #8629, #25161, #13662, .T. ) ;
#9226 = CARTESIAN_POINT ( 'NONE',  ( -290.0000000000001705, -165.0000000000001137, -59.99999999999986500 ) ) ;
#9227 = EDGE_CURVE ( 'NONE', #4314, #17184, #2722, .T. ) ;
#9228 = AXIS2_PLACEMENT_3D ( 'NONE', #10917, #12798, #19250 ) ;
#9229 = LINE ( 'NONE', #17990, #7968 ) ;
#9230 = CARTESIAN_POINT ( 'NONE',  ( -141.6010952119794126, 70.58289405497825442, 82.86345960551251721 ) ) ;
#9231 = ORIENTED_EDGE ( 'NONE', *, *, #1466, .T. ) ;
#9232 = DIRECTION ( 'NONE',  ( 1.000000000000000000, 0.000000000000000000, 0.000000000000000000 ) ) ;
#9233 = EDGE_CURVE ( 'NONE', #17812, #17412, #26035, .T. ) ;
#9234 = ORIENTED_EDGE ( 'NONE', *, *, #12584, .F. ) ;
#9235 = FACE_OUTER_BOUND ( 'NONE', #8351, .T. ) ;
#9236 = LINE ( 'NONE', #13991, #25964 ) ;
#9237 = ORIENTED_EDGE ( 'NONE', *, *, #23333, .F. ) ;
#9238 = EDGE_LOOP ( 'NONE', ( #25407, #6747 ) ) ;
#9239 = LINE ( 'NONE', #7516, #4444 ) ;
#9240 = VECTOR ( 'NONE', #7425, 1000.000000000000000 ) ;
#9241 = CARTESIAN_POINT ( 'NONE',  ( 158.0000000000003695, 171.3503748573662051, -45.00000000000000000 ) ) ;
#9242 = ORIENTED_EDGE ( 'NONE', *, *, #12748, .F. ) ;
#9243 = FACE_OUTER_BOUND ( 'NONE', #2549, .T. ) ;
#9244 = VERTEX_POINT ( 'NONE', #16517 ) ;
#9245 = VECTOR ( 'NONE', #74, 1000.000000000000000 ) ;
#9246 = CARTESIAN_POINT ( 'NONE',  ( -260.0000000000001137, -157.0000000000000284, 110.0000000000000142 ) ) ;
#9247 = VECTOR ( 'NONE', #13366, 1000.000000000000000 ) ;
#9248 = DIRECTION ( 'NONE',  ( 0.000000000000000000, -1.000000000000000000, 0.000000000000000000 ) ) ;
#9249 = CARTESIAN_POINT ( 'NONE',  ( 109.0192378864665557, 205.0000000000002558, -138.9999999999999432 ) ) ;
#9250 = CARTESIAN_POINT ( 'NONE',  ( 5.594927750205532568, 137.4232256183554171, -15.08939307562826215 ) ) ;
#9251 = DIRECTION ( 'NONE',  ( 0.4528218681382713551, 0.8916010070293584056, -0.000000000000000000 ) ) ;
#9252 = CARTESIAN_POINT ( 'NONE',  ( -268.8295757390185940, -165.3167864666411901, -88.70020982224049533 ) ) ;
#9253 = CARTESIAN_POINT ( 'NONE',  ( 158.0000000000008242, 128.2086247222394206, -45.00000000000000000 ) ) ;
#9254 = ORIENTED_EDGE ( 'NONE', *, *, #27843, .T. ) ;
#9255 = LINE ( 'NONE', #2927, #13240 ) ;
#9256 = EDGE_CURVE ( 'NONE', #301, #22565, #18924, .T. ) ;
#9257 = CARTESIAN_POINT ( 'NONE',  ( -210.7172313291012529, 103.7585653882801182, 5.000000000000002665 ) ) ;
#9258 = PLANE ( 'NONE',  #13252 ) ;
#9259 = DIRECTION ( 'NONE',  ( 0.000000000000000000, 0.000000000000000000, 1.000000000000000000 ) ) ;
#9260 = ORIENTED_EDGE ( 'NONE', *, *, #1977, .T. ) ;
#9261 = DIRECTION ( 'NONE',  ( -1.000000000000000000, 0.000000000000000000, 0.000000000000000000 ) ) ;
#9262 = EDGE_CURVE ( 'NONE', #25171, #22044, #7615, .T. ) ;
#9263 = ORIENTED_EDGE ( 'NONE', *, *, #19204, .T. ) ;
#9264 = CIRCLE ( 'NONE', #22574, 43.76444293738737912 ) ;
#9265 = EDGE_CURVE ( 'NONE', #18558, #17461, #27275, .T. ) ;
#9266 = CARTESIAN_POINT ( 'NONE',  ( 134.9999999999998579, 467.1080826427131001, -134.2811822434184705 ) ) ;
#9267 = DIRECTION ( 'NONE',  ( 0.4528218681382713551, 0.8916010070293584056, -0.000000000000000000 ) ) ;
#9268 = CARTESIAN_POINT ( 'NONE',  ( 139.7676321182949835, 249.6195736766799484, -148.6640466283485296 ) ) ;
#9269 = ORIENTED_EDGE ( 'NONE', *, *, #15309, .F. ) ;
#9270 = DIRECTION ( 'NONE',  ( -1.000000000000000000, 0.000000000000000000, -0.000000000000000000 ) ) ;
#9271 = AXIS2_PLACEMENT_3D ( 'NONE', #26602, #331, #24312 ) ;
#9272 = EDGE_LOOP ( 'NONE', ( #23937, #4663, #1864, #24821 ) ) ;
#9273 = AXIS2_PLACEMENT_3D ( 'NONE', #26750, #7221, #20140 ) ;
#9274 = CARTESIAN_POINT ( 'NONE',  ( -124.9781469243919076, 222.2250949724356985, 15.00000000000000000 ) ) ;
#9275 = ORIENTED_EDGE ( 'NONE', *, *, #15309, .T. ) ;
#9276 = CARTESIAN_POINT ( 'NONE',  ( 162.0806940948679085, 180.4841764145329250, -45.00000000000000000 ) ) ;
#9277 = VERTEX_POINT ( 'NONE', #5587 ) ;
#9278 = ORIENTED_EDGE ( 'NONE', *, *, #8607, .T. ) ;
#9279 = DIRECTION ( 'NONE',  ( -0.8916010070300078860, 0.4528218681369924337, 0.000000000000000000 ) ) ;
#9280 = ORIENTED_EDGE ( 'NONE', *, *, #1095, .T. ) ;
#9281 = ORIENTED_EDGE ( 'NONE', *, *, #10879, .F. ) ;
#9282 = EDGE_LOOP ( 'NONE', ( #20896, #2792, #3965, #24796 ) ) ;
#9283 = CARTESIAN_POINT ( 'NONE',  ( 106.7420202941122653, 244.4253804639437533, 31.38183343148724092 ) ) ;
#9284 = VECTOR ( 'NONE', #26889, 1000.000000000000114 ) ;
#9285 = DIRECTION ( 'NONE',  ( -0.8916010070293409751, -0.4528218681383056610, 0.000000000000000000 ) ) ;
#9286 = CARTESIAN_POINT ( 'NONE',  ( 158.0000000000000568, 201.4448749474510407, 45.00000000000000000 ) ) ;
#9287 = VECTOR ( 'NONE', #11884, 1000.000000000000000 ) ;
#9288 = VECTOR ( 'NONE', #8239, 1000.000000000000000 ) ;
#9289 = CARTESIAN_POINT ( 'NONE',  ( 158.0000000000002558, 181.3818748873943889, 45.00000000000000000 ) ) ;
#9290 = EDGE_CURVE ( 'NONE', #16854, #24374, #11933, .T. ) ;
#9291 = DIRECTION ( 'NONE',  ( 0.000000000000000000, -1.000000000000000000, 0.000000000000000000 ) ) ;
#9292 = CARTESIAN_POINT ( 'NONE',  ( 139.9999999999999147, 4.857225732735056709E-14, -70.00000000000001421 ) ) ;
#9293 = CARTESIAN_POINT ( 'NONE',  ( 111.5363082892543218, -5.992022692082500157, -45.00000000000000000 ) ) ;
#9294 = LINE ( 'NONE', #7136, #17677 ) ;
#9295 = CARTESIAN_POINT ( 'NONE',  ( 8.117852850209610338, 141.5785587194356197, -13.00000000000000000 ) ) ;
#9296 = DIRECTION ( 'NONE',  ( -0.5555587585212683477, -0.8314772792026894344, 0.000000000000000000 ) ) ;
#9297 = DIRECTION ( 'NONE',  ( 0.000000000000000000, 0.000000000000000000, -1.000000000000000000 ) ) ;
#9298 = ORIENTED_EDGE ( 'NONE', *, *, #2759, .F. ) ;
#9299 = DIRECTION ( 'NONE',  ( 0.000000000000000000, 0.000000000000000000, 1.000000000000000000 ) ) ;
#9300 = EDGE_CURVE ( 'NONE', #21416, #7297, #7475, .T. ) ;
#9301 = EDGE_CURVE ( 'NONE', #28016, #22498, #1135, .T. ) ;
#9302 = CARTESIAN_POINT ( 'NONE',  ( 157.4999999999998579, 158.5570623160774630, 45.00000000000000000 ) ) ;
#9303 = DIRECTION ( 'NONE',  ( 0.8153095126952284444, -0.5790253867566337309, 0.000000000000000000 ) ) ;
#9304 = CARTESIAN_POINT ( 'NONE',  ( 106.8135592195724826, 209.7270530936113175, -141.9943226514401999 ) ) ;
#9305 = B_SPLINE_CURVE_WITH_KNOTS ( 'NONE', 3,
 ( #1495, #14869, #5669, #23334, #25617, #5526 ),
 .UNSPECIFIED., .F., .F.,
 ( 4, 2, 4 ),
 ( 0.000000000000000000, 0.004615224477119865554, 0.009230448954239731107 ),
 .UNSPECIFIED. ) ;
#9306 = ORIENTED_EDGE ( 'NONE', *, *, #18754, .F. ) ;
#9307 = CIRCLE ( 'NONE', #15728, 7.108535549237485540 ) ;
#9308 = VECTOR ( 'NONE', #20390, 1000.000000000000000 ) ;
#9309 = CARTESIAN_POINT ( 'NONE',  ( 109.5201339680999837, 255.4997179839799060, -37.19466046300052398 ) ) ;
#9310 = ORIENTED_EDGE ( 'NONE', *, *, #14238, .T. ) ;
#9311 = CARTESIAN_POINT ( 'NONE',  ( 157.4999999999998579, 220.0000000000000284, 90.00000000000002842 ) ) ;
#9312 = AXIS2_PLACEMENT_3D ( 'NONE', #8185, #27564, #6026 ) ;
#9313 = VERTEX_POINT ( 'NONE', #12074 ) ;
#9314 = AXIS2_PLACEMENT_3D ( 'NONE', #3248, #16349, #3529 ) ;
#9315 = ORIENTED_EDGE ( 'NONE', *, *, #16567, .F. ) ;
#9316 = VERTEX_POINT ( 'NONE', #20674 ) ;
#9317 = ORIENTED_EDGE ( 'NONE', *, *, #587, .F. ) ;
#9318 = DIRECTION ( 'NONE',  ( -0.000000000000000000, 1.000000000000000000, -0.000000000000000000 ) ) ;
#9319 = CARTESIAN_POINT ( 'NONE',  ( 158.0000000000005116, 160.8109998198309825, -45.00000000000000000 ) ) ;
#9320 = DIRECTION ( 'NONE',  ( -0.4383711467890776259, 0.000000000000000000, 0.8987940462991669266 ) ) ;
#9321 = CARTESIAN_POINT ( 'NONE',  ( -47.47939869681532343, 132.2278273089350762, -14.48490952286894640 ) ) ;
#9322 = ADVANCED_FACE ( 'NONE', ( #27407 ), #7750, .F. ) ;
#9323 = DIRECTION ( 'NONE',  ( -0.8916010070294706491, -0.4528218681380501986, 0.000000000000000000 ) ) ;
#9324 = AXIS2_PLACEMENT_3D ( 'NONE', #3051, #20443, #5353 ) ;
#9325 = CARTESIAN_POINT ( 'NONE',  ( -221.9864287755669068, 60.98533040124961246, 21.67821222924225211 ) ) ;
#9326 = CARTESIAN_POINT ( 'NONE',  ( -40.40953891503691153, 71.03850157808263077, 99.00000000000000000 ) ) ;
#9327 = EDGE_CURVE ( 'NONE', #25161, #18388, #16380, .T. ) ;
#9328 = CARTESIAN_POINT ( 'NONE',  ( 158.0000000000000853, 198.4291249324366504, 45.00000000000000000 ) ) ;
#9329 = CIRCLE ( 'NONE', #25839, 6.000000000000005329 ) ;
#9330 = LINE ( 'NONE', #13081, #25969 ) ;
#9331 = CARTESIAN_POINT ( 'NONE',  ( -231.3807819610386218, 93.01706144896263595, -12.99999999999997691 ) ) ;
#9332 = AXIS2_PLACEMENT_3D ( 'NONE', #21935, #26242, #19502 ) ;
#9333 = CARTESIAN_POINT ( 'NONE',  ( 157.9999999999998010, 241.0630000600560550, 45.00000000000000000 ) ) ;
#9334 = CARTESIAN_POINT ( 'NONE',  ( 158.0000000000009663, 111.1613746771971876, 45.00000000000000000 ) ) ;
#9335 = CARTESIAN_POINT ( 'NONE',  ( 79.99999999999992895, 110.0000000000000000, 70.00000000000001421 ) ) ;
#9336 = CARTESIAN_POINT ( 'NONE',  ( -8.816046456736254200, 132.3922476905560472, 15.94591420432834461 ) ) ;
#9337 = EDGE_CURVE ( 'NONE', #15531, #17645, #9771, .T. ) ;
#9338 = CARTESIAN_POINT ( 'NONE',  ( 11.56692809527929278, 215.3083398198040470, 45.00000000000000000 ) ) ;
#9339 = CARTESIAN_POINT ( 'NONE',  ( 187.4999999999996305, 258.6181251126050711, 6.000000000000019540 ) ) ;
#9340 = CARTESIAN_POINT ( 'NONE',  ( 232.4999999999996305, 83.06687458711267880, -30.83984227207693607 ) ) ;
#9342 = ORIENTED_EDGE ( 'NONE', *, *, #22508, .T. ) ;
#9341 = EDGE_LOOP ( 'NONE', ( #2863, #24651, #22659, #15533, #18974 ) ) ;
#9343 = FACE_OUTER_BOUND ( 'NONE', #22702, .T. ) ;
#9344 = ADVANCED_FACE ( 'NONE', ( #14365 ), #14226, .F. ) ;
#9345 = DIRECTION ( 'NONE',  ( 1.000000000000000000, -0.000000000000000000, -0.000000000000000000 ) ) ;
#9346 = ORIENTED_EDGE ( 'NONE', *, *, #11995, .T. ) ;
#9347 = ITEM_DEFINED_TRANSFORMATION ( 'NONE', 'NONE', #5139,  #10637 ) ;
#9348 = EDGE_LOOP ( 'NONE', ( #18552, #18045, #17219, #24251 ) ) ;
#9349 = VECTOR ( 'NONE', #17501, 1000.000000000000000 ) ;
#9350 = ORIENTED_EDGE ( 'NONE', *, *, #19705, .F. ) ;
#9351 = AXIS2_PLACEMENT_3D ( 'NONE', #5047, #7504, #22587 ) ;
#9352 = DIRECTION ( 'NONE',  ( -1.000000000000000000, 0.000000000000000000, 2.775557561562887407E-16 ) ) ;
#9353 = CARTESIAN_POINT ( 'NONE',  ( -135.2491457716903653, 129.6667746786781947, 15.43809234620010962 ) ) ;
#9354 = ORIENTED_EDGE ( 'NONE', *, *, #11508, .F. ) ;
#9355 = CIRCLE ( 'NONE', #14396, 5.999999999999977796 ) ;
#9356 = ORIENTED_EDGE ( 'NONE', *, *, #18501, .T. ) ;
#9357 = CARTESIAN_POINT ( 'NONE',  ( 158.0000000000016769, 47.95662448201407102, 45.00000000000000000 ) ) ;
#9358 = EDGE_CURVE ( 'NONE', #14502, #25694, #14088, .T. ) ;
#9359 = DIRECTION ( 'NONE',  ( -1.000000000000000000, 0.000000000000000000, 0.000000000000000000 ) ) ;
#9360 = DIRECTION ( 'NONE',  ( 1.000000000000000000, 8.759632170410045475E-15, 0.000000000000000000 ) ) ;
#9361 = ORIENTED_EDGE ( 'NONE', *, *, #7519, .T. ) ;
#9362 = DIRECTION ( 'NONE',  ( -0.000000000000000000, -0.000000000000000000, -1.000000000000000000 ) ) ;
#9363 =( BOUNDED_SURFACE ( )  B_SPLINE_SURFACE ( 3, 2, ( 
 ( #4994, #5287, #18509 ),
 ( #27254, #1117, #9321 ),
 ( #7308, #24833, #22820 ),
 ( #14207, #22956, #26976 ),
 ( #22682, #3260, #20374 ),
 ( #20517, #27388, #9886 ),
 ( #7452, #12197, #16222 ),
 ( #14069, #3120, #18644 ),
 ( #7730, #2984, #16498 ),
 ( #25250, #14344, #3404 ),
 ( #11775, #559, #18085 ),
 ( #13787, #22534, #2844 ),
 ( #703, #9472, #18229 ),
 ( #16082, #5143, #6272 ),
 ( #25808, #17049, #23665 ),
 ( #23517, #12758, #14909 ),
 ( #27810, #3970, #6133 ),
 ( #23376, #10168, #1397 ),
 ( #21497, #18927, #3685 ),
 ( #16776, #1815, #28095 ),
 ( #8148, #19343, #21217 ),
 ( #15046, #25665, #10590 ),
 ( #18783, #16911, #12620 ),
 ( #3830, #8438, #1258 ),
 ( #27669, #25528, #14764 ),
 ( #21359, #17192, #25951 ),
 ( #20937, #23803, #1677 ),
 ( #4113, #10447, #10027 ) ),
 .UNSPECIFIED., .F., .F., .F. ) 
 B_SPLINE_SURFACE_WITH_KNOTS ( ( 4, 2, 2, 2, 2, 2, 2, 2, 2, 2, 2, 2, 2, 4 ),
 ( 3, 3 ),
 ( -6.071532165918824830E-18, 0.01498678567651468181, 0.02997357135302937056, 0.04496035702954406105, 0.05245374986780140802, 0.05620044628693007804, 0.05994714270605874806, 0.07493392838257342814, 0.08992071405908812209, 0.09741410689734547601, 0.1049074997356028160, 0.1086541961547314861, 0.1124008925738601561, 0.1198942854121174961 ),
 ( 0.000000000000000000, 1.000000000000000000 ),
 .UNSPECIFIED. ) 
 GEOMETRIC_REPRESENTATION_ITEM ( )  RATIONAL_B_SPLINE_SURFACE ( (
 ( 1.000000000000000000, 0.8161343730438194166, 1.000000000000000000),
 ( 1.000000000000000000, 0.8053590984426869381, 1.000000000000000000),
 ( 1.000000000000000000, 0.7960137040925352458, 1.000000000000000000),
 ( 1.000000000000000000, 0.7808453201752241224, 1.000000000000000000),
 ( 1.000000000000000000, 0.7750273194348902273, 1.000000000000000000),
 ( 1.000000000000000000, 0.7674151632800794154, 1.000000000000000000),
 ( 1.000000000000000000, 0.7656231679750936658, 1.000000000000000000),
 ( 1.000000000000000000, 0.7661290450854815193, 1.000000000000000000),
 ( 1.000000000000000000, 0.7668277142013406600, 1.000000000000000000),
 ( 1.000000000000000000, 0.7686712949395471117, 1.000000000000000000),
 ( 1.000000000000000000, 0.7694194103377227645, 1.000000000000000000),
 ( 1.000000000000000000, 0.7711707737263995277, 1.000000000000000000),
 ( 1.000000000000000000, 0.7721740736493929447, 1.000000000000000000),
 ( 1.000000000000000000, 0.7778076735771930483, 1.000000000000000000),
 ( 1.000000000000000000, 0.7842969395606893546, 1.000000000000000000),
 ( 1.000000000000000000, 0.8005680270097221829, 1.000000000000000000),
 ( 1.000000000000000000, 0.8103469025248568602, 1.000000000000000000),
 ( 1.000000000000000000, 0.8268680461880919541, 1.000000000000000000),
 ( 1.000000000000000000, 0.8326830769007559363, 1.000000000000000000),
 ( 1.000000000000000000, 0.8448194715605038541, 1.000000000000000000),
 ( 1.000000000000000000, 0.8511408365003451104, 1.000000000000000000),
 ( 1.000000000000000000, 0.8609175397525088425, 1.000000000000000000),
 ( 1.000000000000000000, 0.8642255213344454123, 1.000000000000000000),
 ( 1.000000000000000000, 0.8709250352162014597, 1.000000000000000000),
 ( 1.000000000000000000, 0.8743096907132095197, 1.000000000000000000),
 ( 1.000000000000000000, 0.8844861762812324946, 1.000000000000000000),
 ( 1.000000000000000000, 0.8913208799372495106, 1.000000000000000000),
 ( 1.000000000000000000, 0.8981184559478653240, 1.000000000000000000) ) ) 
 REPRESENTATION_ITEM ( '' )  SURFACE ( )  );
#9364 = DIRECTION ( 'NONE',  ( 1.000000000000000000, 0.000000000000000000, 0.000000000000000000 ) ) ;
#9365 = ADVANCED_FACE ( 'NONE', ( #18387 ), #5307, .F. ) ;
#9366 = DIRECTION ( 'NONE',  ( -0.000000000000000000, -0.000000000000000000, -1.000000000000000000 ) ) ;
#9367 = DIRECTION ( 'NONE',  ( 1.000000000000000000, 1.530283246943720875E-16, 0.000000000000000000 ) ) ;
#9368 = CARTESIAN_POINT ( 'NONE',  ( -215.3445465745174658, 71.74628434702670177, -26.24848034640785954 ) ) ;
#9369 = AXIS2_PLACEMENT_3D ( 'NONE', #6592, #6448, #25984 ) ;
#9370 = ORIENTED_EDGE ( 'NONE', *, *, #10835, .T. ) ;
#9371 = DIRECTION ( 'NONE',  ( -1.000000000000000000, -1.530283246943720875E-16, 0.000000000000000000 ) ) ;
#9372 = CARTESIAN_POINT ( 'NONE',  ( -215.4886702565632675, 139.8420026707765942, -15.00000000000000178 ) ) ;
#9373 = DIRECTION ( 'NONE',  ( 1.000000000000000000, 0.000000000000000000, 0.000000000000000000 ) ) ;
#9374 = AXIS2_PLACEMENT_3D ( 'NONE', #20842, #22999, #23535 ) ;
#9375 = LINE ( 'NONE', #7214, #25879 ) ;
#9376 = ORIENTED_EDGE ( 'NONE', *, *, #13189, .T. ) ;
#9377 = DIRECTION ( 'NONE',  ( 0.6681556583950127859, 0.7440215159219033536, 0.000000000000000000 ) ) ;
#9378 = EDGE_CURVE ( 'NONE', #14926, #18830, #7883, .T. ) ;
#9379 = EDGE_CURVE ( 'NONE', #8966, #6472, #4233, .T. ) ;
#9380 = CYLINDRICAL_SURFACE ( 'NONE', #13959, 2.586968381275096984 ) ;
#9381 = DIRECTION ( 'NONE',  ( 0.000000000000000000, -1.000000000000000000, 0.000000000000000000 ) ) ;
#9382 = VERTEX_POINT ( 'NONE', #22838 ) ;
#9383 = VERTEX_POINT ( 'NONE', #3564 ) ;
#9384 = CARTESIAN_POINT ( 'NONE',  ( 108.2273028577272385, 129.5338070839680711, 99.99999999997838529 ) ) ;
#9385 = LINE ( 'NONE', #26901, #13126 ) ;
#9386 = VERTEX_POINT ( 'NONE', #21095 ) ;
#9387 = AXIS2_PLACEMENT_3D ( 'NONE', #316, #13681, #13249 ) ;
#9389 = EDGE_CURVE ( 'NONE', #13728, #14325, #18945, .T. ) ;
#9388 = ORIENTED_EDGE ( 'NONE', *, *, #22266, .T. ) ;
#9390 = DIRECTION ( 'NONE',  ( 1.000000000000000000, 0.000000000000000000, 0.000000000000000000 ) ) ;
#9391 = LINE ( 'NONE', #3184, #25396 ) ;
#9392 = ORIENTED_EDGE ( 'NONE', *, *, #10352, .F. ) ;
#9393 = CARTESIAN_POINT ( 'NONE',  ( 167.4999999999996589, -5.589247009368136787, -84.99999999999995737 ) ) ;
#9394 = ORIENTED_EDGE ( 'NONE', *, *, #10266, .T. ) ;
#9395 = VECTOR ( 'NONE', #5270, 1000.000000000000227 ) ;
#9396 = CARTESIAN_POINT ( 'NONE',  ( 145.9999999999998863, 220.0000000000000284, 100.0000000000000142 ) ) ;
#9397 = EDGE_CURVE ( 'NONE', #5476, #9639, #27689, .T. ) ;
#9398 = CARTESIAN_POINT ( 'NONE',  ( 157.4999999999998579, 75.79718706834503905, -45.00000000000000000 ) ) ;
#9399 = ADVANCED_FACE ( 'NONE', ( #22701 ), #4390, .T. ) ;
#9400 = DIRECTION ( 'NONE',  ( -0.000000000000000000, -0.000000000000000000, -1.000000000000000000 ) ) ;
#9401 = CARTESIAN_POINT ( 'NONE',  ( -5.362442292600443139, 133.6996795038672587, -14.05115172523858469 ) ) ;
#9402 = LINE ( 'NONE', #22466, #9990 ) ;
#9403 = CARTESIAN_POINT ( 'NONE',  ( -266.9577532651693446, -165.5716054493118463, -89.18913380684575998 ) ) ;
#9404 = DIRECTION ( 'NONE',  ( -0.000000000000000000, -0.000000000000000000, 1.000000000000000000 ) ) ;
#9405 = ORIENTED_EDGE ( 'NONE', *, *, #23823, .T. ) ;
#9406 = DIRECTION ( 'NONE',  ( -0.000000000000000000, -0.000000000000000000, -1.000000000000000000 ) ) ;
#9407 = DIRECTION ( 'NONE',  ( 1.040834085586083310E-14, 0.000000000000000000, 1.000000000000000000 ) ) ;
#9408 = DIRECTION ( 'NONE',  ( 0.8018642810807392607, 0.5975062131282562472, 0.000000000000000000 ) ) ;
#9409 = CARTESIAN_POINT ( 'NONE',  ( 157.9999999999997726, 246.0787500750700474, -45.00000000000000000 ) ) ;
#9410 = EDGE_LOOP ( 'NONE', ( #7118, #20812, #24187, #470 ) ) ;
#9411 = AXIS2_PLACEMENT_3D ( 'NONE', #26694, #12933, #17655 ) ;
#9412 = CARTESIAN_POINT ( 'NONE',  ( -243.4285414610288001, 74.63108012613848530, 5.000000000000001776 ) ) ;
#9413 = ORIENTED_EDGE ( 'NONE', *, *, #22140, .T. ) ;
#9414 = FACE_OUTER_BOUND ( 'NONE', #10038, .T. ) ;
#9415 = CARTESIAN_POINT ( 'NONE',  ( -234.1469129038715096, 66.78385994367806688, -6.149209796590396238 ) ) ;
#9416 = CARTESIAN_POINT ( 'NONE',  ( 141.0001535789425020, 249.3938455642302756, -144.6099047286054713 ) ) ;
#9417 = ORIENTED_EDGE ( 'NONE', *, *, #2225, .F. ) ;
#9418 = LINE ( 'NONE', #20606, #26682 ) ;
#9419 = FACE_OUTER_BOUND ( 'NONE', #18110, .T. ) ;
#9420 = EDGE_CURVE ( 'NONE', #7851, #16902, #13340, .T. ) ;
#9421 = TOROIDAL_SURFACE ( 'NONE', #3428, 35.00000000000000711, 5.000000000000000000 ) ;
#9422 = VERTEX_POINT ( 'NONE', #24381 ) ;
#9423 = CARTESIAN_POINT ( 'NONE',  ( -43.02437977270766822, 129.7200458115292747, 16.81627168235289815 ) ) ;
#9424 = VERTEX_POINT ( 'NONE', #19785 ) ;
#9425 = DIRECTION ( 'NONE',  ( 8.659560562354934091E-17, 0.7071067811865474617, -0.7071067811865476838 ) ) ;
#9426 = VERTEX_POINT ( 'NONE', #22376 ) ;
#9427 = VERTEX_POINT ( 'NONE', #26827 ) ;
#9428 = PLANE ( 'NONE',  #25088 ) ;
#9429 = ORIENTED_EDGE ( 'NONE', *, *, #8505, .F. ) ;
#9430 = VECTOR ( 'NONE', #5813, 1000.000000000000000 ) ;
#9431 = VERTEX_POINT ( 'NONE', #26254 ) ;
#9432 = VERTEX_POINT ( 'NONE', #4981 ) ;
#9433 = VECTOR ( 'NONE', #15053, 1000.000000000000000 ) ;
#9434 = ADVANCED_FACE ( 'NONE', ( #22231 ), #20217, .F. ) ;
#9435 = CARTESIAN_POINT ( 'NONE',  ( 96.29556199549340079, 241.0127520899143576, 10.03785181564020235 ) ) ;
#9436 = EDGE_CURVE ( 'NONE', #20572, #21229, #3799, .T. ) ;
#9437 = CARTESIAN_POINT ( 'NONE',  ( -42.99650729631200363, 36.92584315232891612, 100.0000000000000000 ) ) ;
#9438 = CARTESIAN_POINT ( 'NONE',  ( -56.48697296830715686, 1.968917815184006985E-15, 99.00000000000000000 ) ) ;
#9439 = VECTOR ( 'NONE', #5616, 1000.000000000000000 ) ;
#9440 = CARTESIAN_POINT ( 'NONE',  ( 100.5794065449870942, 118.1137289701970872, -81.24999999966573228 ) ) ;
#9441 = PLANE ( 'NONE',  #8989 ) ;
#9442 = LINE ( 'NONE', #15913, #5161 ) ;
#9443 = LINE ( 'NONE', #3093, #7197 ) ;
#9444 = PLANE ( 'NONE',  #3912 ) ;
#9445 = LINE ( 'NONE', #27363, #7422 ) ;
#9446 = CARTESIAN_POINT ( 'NONE',  ( -79.00187704905530950, 96.44595867864546790, -145.0000000000000000 ) ) ;
#9447 = CARTESIAN_POINT ( 'NONE',  ( -180.0000000000000284, -70.00000000000004263, -25.00000000000000000 ) ) ;
#9448 = ORIENTED_EDGE ( 'NONE', *, *, #8578, .F. ) ;
#9449 = DIRECTION ( 'NONE',  ( 0.000000000000000000, -1.000000000000000000, 0.000000000000000000 ) ) ;
#9450 = ADVANCED_FACE ( 'NONE', ( #19931 ), #17772, .F. ) ;
#9451 = CARTESIAN_POINT ( 'NONE',  ( -17.24491960465746132, 75.97823757117562593, 100.0000000000000000 ) ) ;
#9452 = DIRECTION ( 'NONE',  ( -1.000000000000000000, 0.000000000000000000, 0.000000000000000000 ) ) ;
#9453 = VECTOR ( 'NONE', #20159, 1000.000000000000000 ) ;
#9454 = DIRECTION ( 'NONE',  ( 0.000000000000000000, -1.000000000000000000, 0.000000000000000000 ) ) ;
#9455 = ORIENTED_EDGE ( 'NONE', *, *, #3406, .T. ) ;
#9456 = AXIS2_PLACEMENT_3D ( 'NONE', #8104, #5521, #1630 ) ;
#9457 = CARTESIAN_POINT ( 'NONE',  ( 109.9999999999998863, 260.0000000000000000, -45.00000000000000000 ) ) ;
#9458 = VERTEX_POINT ( 'NONE', #13773 ) ;
#9459 = EDGE_CURVE ( 'NONE', #19265, #24488, #11327, .T. ) ;
#9460 = LINE ( 'NONE', #18217, #6790 ) ;
#9461 = VECTOR ( 'NONE', #14489, 1000.000000000000000 ) ;
#9462 = VERTEX_POINT ( 'NONE', #690 ) ;
#9463 = EDGE_LOOP ( 'NONE', ( #12843, #12665, #24220 ) ) ;
#9464 = EDGE_LOOP ( 'NONE', ( #2509, #21032, #20003, #24207 ) ) ;
#9465 = EDGE_CURVE ( 'NONE', #4554, #5560, #6579, .T. ) ;
#9466 = ORIENTED_EDGE ( 'NONE', *, *, #21572, .F. ) ;
#9467 = LINE ( 'NONE', #22384, #3543 ) ;
#9468 = LINE ( 'NONE', #22242, #9527 ) ;
#9469 = DIRECTION ( 'NONE',  ( -0.000000000000000000, -0.000000000000000000, -1.000000000000000000 ) ) ;
#9470 = EDGE_CURVE ( 'NONE', #21067, #23466, #23540, .T. ) ;
#9471 = EDGE_CURVE ( 'NONE', #19742, #7009, #26671, .T. ) ;
#9472 = CARTESIAN_POINT ( 'NONE',  ( -101.6427404889548711, 135.8129376563426831, -15.24817990273632340 ) ) ;
#9473 = AXIS2_PLACEMENT_3D ( 'NONE', #21984, #8635, #17390 ) ;
#9474 = DIRECTION ( 'NONE',  ( 1.000000000000000000, 0.000000000000000000, 0.000000000000000000 ) ) ;
#9475 = CARTESIAN_POINT ( 'NONE',  ( -213.2464434226970980, 57.29534669709770611, 37.98348409338887421 ) ) ;
#9476 = CARTESIAN_POINT ( 'NONE',  ( -261.1919288306253293, -171.9377729149742038, 105.0000000000000142 ) ) ;
#9477 = CARTESIAN_POINT ( 'NONE',  ( -42.53273978471831640, 130.9733465240572627, -14.93735646117640492 ) ) ;
#9478 = CARTESIAN_POINT ( 'NONE',  ( -63.57415822541634043, 24.64876300893806160, 95.00000000000000000 ) ) ;
#9479 = CARTESIAN_POINT ( 'NONE',  ( -225.7503879793210899, 89.48004551377478322, -13.96212495524699015 ) ) ;
#9480 = AXIS2_PLACEMENT_3D ( 'NONE', #19173, #27643, #1649 ) ;
#9481 = CARTESIAN_POINT ( 'NONE',  ( 167.4999999999996589, 526.4263741777961059, -74.99999999999995737 ) ) ;
#9482 = CARTESIAN_POINT ( 'NONE',  ( 157.9999999999996305, 286.2047501951820436, -45.00000000000000000 ) ) ;
#9483 = CARTESIAN_POINT ( 'NONE',  ( 105.2480867101079980, 123.6573351780392613, 85.93750000029402258 ) ) ;
#9484 = CARTESIAN_POINT ( 'NONE',  ( -23.59768067310782413, 129.3237483323889592, 16.93303552989647898 ) ) ;
#9485 = DIRECTION ( 'NONE',  ( -0.9985600561963492439, -0.05364526231778203591, 0.000000000000000000 ) ) ;
#9486 = CARTESIAN_POINT ( 'NONE',  ( 157.4999999999998579, 110.9074371734436255, 45.00000000000000000 ) ) ;
#9487 = CARTESIAN_POINT ( 'NONE',  ( -63.57415822541634043, -23.01420295945612082, 80.00000000000001421 ) ) ;
#9489 = ORIENTED_EDGE ( 'NONE', *, *, #23404, .T. ) ;
#9488 = VERTEX_POINT ( 'NONE', #7000 ) ;
#9490 = DIRECTION ( 'NONE',  ( 0.8916010070300282031, -0.4528218681369524101, 0.000000000000000000 ) ) ;
#9491 = DIRECTION ( 'NONE',  ( -1.000000000000000000, -1.321694076934710155E-16, 0.000000000000000000 ) ) ;
#9492 = EDGE_LOOP ( 'NONE', ( #8909, #6266, #7414, #3533 ) ) ;
#9493 = VECTOR ( 'NONE', #22492, 1000.000000000000000 ) ;
#9494 = VERTEX_POINT ( 'NONE', #6715 ) ;
#9495 = ADVANCED_FACE ( 'NONE', ( #15497 ), #18494, .F. ) ;
#9496 = EDGE_CURVE ( 'NONE', #5842, #10608, #6557, .T. ) ;
#9497 = CARTESIAN_POINT ( 'NONE',  ( 157.9999999999997158, 256.6181251126050711, 45.00000000000000000 ) ) ;
#9498 = CARTESIAN_POINT ( 'NONE',  ( -138.3093778148924571, 127.5098211573111087, 17.72095338322215952 ) ) ;
#9499 = VERTEX_POINT ( 'NONE', #13919 ) ;
#9500 = ORIENTED_EDGE ( 'NONE', *, *, #20647, .F. ) ;
#9501 = DIRECTION ( 'NONE',  ( 0.8916010070293584056, -0.4528218681382712996, 0.000000000000000000 ) ) ;
#9502 = PLANE ( 'NONE',  #3992 ) ;
#9503 = EDGE_CURVE ( 'NONE', #20254, #15707, #16654, .T. ) ;
#9504 = DIRECTION ( 'NONE',  ( -0.8916010070293383105, -0.4528218681383106015, 0.000000000000000000 ) ) ;
#9505 = CARTESIAN_POINT ( 'NONE',  ( 157.9999999999998579, 221.0000000000000284, 45.00000000000000000 ) ) ;
#9506 = CARTESIAN_POINT ( 'NONE',  ( 89.55287500703019532, 230.0961521423384113, -16.54242257938075156 ) ) ;
#9507 = ADVANCED_FACE ( 'NONE', ( #1103 ), #3104, .F. ) ;
#9508 = DIRECTION ( 'NONE',  ( -1.000000000000000000, 0.000000000000000000, -0.000000000000000000 ) ) ;
#9509 = DIRECTION ( 'NONE',  ( -0.8916010070297746282, 0.4528218681374520105, 0.000000000000000000 ) ) ;
#9510 = CIRCLE ( 'NONE', #11811, 39.99999999999999289 ) ;
#9511 = CARTESIAN_POINT ( 'NONE',  ( -194.7277720219268815, 63.01928361507884091, -39.96465835449415493 ) ) ;
#9512 = AXIS2_PLACEMENT_3D ( 'NONE', #18079, #7304, #20792 ) ;
#9513 = DIRECTION ( 'NONE',  ( -1.000000000000000000, 0.000000000000000000, 0.000000000000000000 ) ) ;
#9514 = LINE ( 'NONE', #13396, #19309 ) ;
#9515 = DIRECTION ( 'NONE',  ( 0.000000000000000000, -1.000000000000000000, 0.000000000000000000 ) ) ;
#9516 = DIRECTION ( 'NONE',  ( 0.8916010070293384215, 0.4528218681383106015, 0.000000000000000000 ) ) ;
#9517 = VERTEX_POINT ( 'NONE', #14059 ) ;
#9518 = LINE ( 'NONE', #27298, #14218 ) ;
#9519 = CARTESIAN_POINT ( 'NONE',  ( -243.5753208290495309, 74.80993601160373885, 14.84129168367922702 ) ) ;
#9520 = CARTESIAN_POINT ( 'NONE',  ( -160.0000000000000568, 90.00000000000001421, 98.28427124746191623 ) ) ;
#9521 = EDGE_LOOP ( 'NONE', ( #18846, #11506, #521, #4057 ) ) ;
#9522 = ORIENTED_EDGE ( 'NONE', *, *, #27821, .T. ) ;
#9523 = EDGE_CURVE ( 'NONE', #17073, #8883, #22942, .T. ) ;
#9524 = CARTESIAN_POINT ( 'NONE',  ( 90.17595424772805757, 111.7661400908348384, 72.22656249985354293 ) ) ;
#9525 = CARTESIAN_POINT ( 'NONE',  ( -202.5288808976002599, 93.61334720101866935, -29.67947843847759870 ) ) ;
#9526 = ORIENTED_EDGE ( 'NONE', *, *, #10051, .T. ) ;
#9527 = VECTOR ( 'NONE', #24393, 1000.000000000000000 ) ;
#9528 = ORIENTED_EDGE ( 'NONE', *, *, #9732, .T. ) ;
#9529 = DIRECTION ( 'NONE',  ( 0.000000000000000000, -1.000000000000000000, 0.000000000000000000 ) ) ;
#9530 = CARTESIAN_POINT ( 'NONE',  ( 158.0000000000005684, 151.2873747973098659, 45.00000000000000000 ) ) ;
#9531 = CARTESIAN_POINT ( 'NONE',  ( 157.4999999999998579, 135.9861872485140850, -45.00000000000000000 ) ) ;
#9532 = ORIENTED_EDGE ( 'NONE', *, *, #10332, .F. ) ;
#9533 = CARTESIAN_POINT ( 'NONE',  ( 217.4999999999996305, 133.0668745871126930, 42.86484227207692044 ) ) ;
#9534 = EDGE_LOOP ( 'NONE', ( #18774, #19196 ) ) ;
#9535 = DIRECTION ( 'NONE',  ( 0.8916010070297037959, -0.4528218681375912325, 0.000000000000000000 ) ) ;
#9536 = ADVANCED_FACE ( 'NONE', ( #16483 ), #16210, .F. ) ;
#9537 = EDGE_CURVE ( 'NONE', #21780, #4389, #11763, .T. ) ;
#9538 = DIRECTION ( 'NONE',  ( -1.000000000000000000, 4.540956701092242152E-16, 0.000000000000000000 ) ) ;
#9539 = DIRECTION ( 'NONE',  ( 0.4999999999999919509, -0.8660254037844432595, -0.000000000000000000 ) ) ;
#9540 = CARTESIAN_POINT ( 'NONE',  ( -25.32102446532049811, 128.0228448628550098, -17.49457884177929046 ) ) ;
#9541 = DIRECTION ( 'NONE',  ( 0.8916010070297041290, 0.4528218681375906218, 0.000000000000000000 ) ) ;
#9542 = PLANE ( 'NONE',  #25272 ) ;
#9543 = CARTESIAN_POINT ( 'NONE',  ( -196.7918453702777128, 68.51688903468615877, 83.00000000000001421 ) ) ;
#9544 = CIRCLE ( 'NONE', #15058, 562.1290781602207289 ) ;
#9545 = VERTEX_POINT ( 'NONE', #14469 ) ;
#9546 = DIRECTION ( 'NONE',  ( -0.5773502691896246208, -0.5773502691896247319, 0.5773502691896278405 ) ) ;
#9547 = CARTESIAN_POINT ( 'NONE',  ( 157.4999999999998579, 221.2539375037535194, 45.00000000000000000 ) ) ;
#9548 = DIRECTION ( 'NONE',  ( 0.4528218681378310406, 0.8916010070295820045, -0.000000000000000000 ) ) ;
#9549 = DIRECTION ( 'NONE',  ( 0.8916010070299470458, -0.4528218681371123377, 0.000000000000000000 ) ) ;
#9550 = ORIENTED_EDGE ( 'NONE', *, *, #24633, .F. ) ;
#9551 = EDGE_CURVE ( 'NONE', #23853, #2800, #24820, .T. ) ;
#9552 = CARTESIAN_POINT ( 'NONE',  ( 157.4999999999998579, 123.4468122109788482, 45.00000000000000000 ) ) ;
#9553 = ORIENTED_EDGE ( 'NONE', *, *, #26309, .F. ) ;
#9554 = EDGE_CURVE ( 'NONE', #6691, #25965, #18770, .T. ) ;
#9555 = DIRECTION ( 'NONE',  ( -0.000000000000000000, -0.000000000000000000, -1.000000000000000000 ) ) ;
#9556 = CARTESIAN_POINT ( 'NONE',  ( 134.9999999999998579, 220.0000000000000284, 99.00000000000001421 ) ) ;
#9557 = CARTESIAN_POINT ( 'NONE',  ( 136.5548239485688953, 249.9602781967704743, -150.7983993365949971 ) ) ;
#9558 = ORIENTED_EDGE ( 'NONE', *, *, #1241, .F. ) ;
#9559 = DIRECTION ( 'NONE',  ( 0.8916010070298961976, -0.4528218681372121468, 0.000000000000000000 ) ) ;
#9560 = DIRECTION ( 'NONE',  ( -0.8916010070293510781, 0.4528218681382856214, 0.000000000000000000 ) ) ;
#9561 = ORIENTED_EDGE ( 'NONE', *, *, #24879, .F. ) ;
#9562 = CARTESIAN_POINT ( 'NONE',  ( 89.99999999999994316, -90.00000000000001421, 100.0000000000000142 ) ) ;
#9563 = CARTESIAN_POINT ( 'NONE',  ( -271.9747264835629608, -170.1913680348071409, -103.5087831302661812 ) ) ;
#9564 = EDGE_LOOP ( 'NONE', ( #27333, #1746 ) ) ;
#9565 = ADVANCED_FACE ( 'NONE', ( #5553 ), #22807, .T. ) ;
#9566 = ORIENTED_EDGE ( 'NONE', *, *, #28214, .F. ) ;
#9567 = DIRECTION ( 'NONE',  ( -0.8660254037844362651, 0.5000000000000039968, 0.000000000000000000 ) ) ;
#9568 = ORIENTED_EDGE ( 'NONE', *, *, #6042, .F. ) ;
#9569 = CONICAL_SURFACE ( 'NONE', #8649, 21.20097097723064294, 0.08885387018394180769 ) ;
#9570 = VECTOR ( 'NONE', #9406, 1000.000000000000000 ) ;
#9571 = ORIENTED_EDGE ( 'NONE', *, *, #27885, .F. ) ;
#9572 = ORIENTED_EDGE ( 'NONE', *, *, #5425, .T. ) ;
#9573 = CARTESIAN_POINT ( 'NONE',  ( 109.9760533923134744, 258.8696700914142070, 43.04221176963723394 ) ) ;
#9574 = DIRECTION ( 'NONE',  ( 0.2066290158914672881, 0.9784193629480785193, 0.000000000000000000 ) ) ;
#9575 = DIRECTION ( 'NONE',  ( 0.000000000000000000, 0.000000000000000000, -1.000000000000000000 ) ) ;
#9576 = CARTESIAN_POINT ( 'NONE',  ( -175.0000000000000000, -120.0000000000001847, -63.97499999999998721 ) ) ;
#9577 = CARTESIAN_POINT ( 'NONE',  ( 134.9999999999998579, 220.0000000000000284, -100.0000000000000142 ) ) ;
#9578 = DIRECTION ( 'NONE',  ( -0.8916010070293515222, 0.4528218681382848443, 0.000000000000000000 ) ) ;
#9579 = VECTOR ( 'NONE', #12937, 1000.000000000000000 ) ;
#9580 = CARTESIAN_POINT ( 'NONE',  ( 157.4999999999998579, 201.1909374436971802, 45.00000000000000000 ) ) ;
#9581 = DIRECTION ( 'NONE',  ( -0.8916010070295820045, -0.4528218681378310406, 0.000000000000000000 ) ) ;
#9582 = CARTESIAN_POINT ( 'NONE',  ( -156.8436863811591593, 180.7779002010535692, -13.00000000000000000 ) ) ;
#9583 = CARTESIAN_POINT ( 'NONE',  ( 157.9999999999997442, 254.1102501050980322, 45.00000000000000000 ) ) ;
#9584 = DIRECTION ( 'NONE',  ( 0.4528218681381102617, -0.8916010070294402290, 0.000000000000000000 ) ) ;
#9585 = ORIENTED_EDGE ( 'NONE', *, *, #20503, .T. ) ;
#9586 = VECTOR ( 'NONE', #20633, 1000.000000000000000 ) ;
#9587 = VECTOR ( 'NONE', #7312, 1000.000000000000000 ) ;
#9588 = CARTESIAN_POINT ( 'NONE',  ( 116.5224093497742786, 212.3463313526978595, -45.00000000000000000 ) ) ;
#9589 = DIRECTION ( 'NONE',  ( 1.000000000000000000, 0.000000000000000000, -3.053113317719176147E-15 ) ) ;
#9590 = PLANE ( 'NONE',  #6937 ) ;
#9591 = ORIENTED_EDGE ( 'NONE', *, *, #12972, .F. ) ;
#9592 = EDGE_CURVE ( 'NONE', #4340, #13994, #5273, .T. ) ;
#9594 = EDGE_CURVE ( 'NONE', #8173, #21166, #27516, .T. ) ;
#9593 = VECTOR ( 'NONE', #2444, 1000.000000000000114 ) ;
#9595 = LINE ( 'NONE', #18215, #12088 ) ;
#9596 = ORIENTED_EDGE ( 'NONE', *, *, #14518, .T. ) ;
#9597 = FILL_AREA_STYLE_COLOUR ( '', #3118 ) ;
#9598 = EDGE_CURVE ( 'NONE', #4619, #14425, #23087, .T. ) ;
#9599 = ORIENTED_EDGE ( 'NONE', *, *, #8931, .T. ) ;
#9600 = VECTOR ( 'NONE', #1340, 1000.000000000000000 ) ;
#9601 = VERTEX_POINT ( 'NONE', #27242 ) ;
#9602 = ORIENTED_EDGE ( 'NONE', *, *, #23793, .T. ) ;
#9603 = ORIENTED_EDGE ( 'NONE', *, *, #14198, .F. ) ;
#9604 = CARTESIAN_POINT ( 'NONE',  ( -108.0099734903331807, 135.2217844244274545, 13.71957698657085345 ) ) ;
#9605 = DIRECTION ( 'NONE',  ( 0.4528218681376712240, 0.8916010070296632728, -0.000000000000000000 ) ) ;
#9606 = DIRECTION ( 'NONE',  ( 0.000000000000000000, 0.000000000000000000, 1.000000000000000000 ) ) ;
#9607 = CIRCLE ( 'NONE', #4516, 6.204828372381208546 ) ;
#9608 = DIRECTION ( 'NONE',  ( -0.000000000000000000, -0.000000000000000000, -1.000000000000000000 ) ) ;
#9609 = CARTESIAN_POINT ( 'NONE',  ( -27.00683456900459234, 129.1643779576224063, 15.68707256237481928 ) ) ;
#9610 = AXIS2_PLACEMENT_3D ( 'NONE', #23696, #27702, #17081 ) ;
#9611 = CARTESIAN_POINT ( 'NONE',  ( -194.6040764069587112, 63.06822542404761123, 40.63350569893458442 ) ) ;
#9612 = DIRECTION ( 'NONE',  ( 0.000000000000000000, 0.000000000000000000, 1.000000000000000000 ) ) ;
#9613 = CARTESIAN_POINT ( 'NONE',  ( 157.9999999999996589, 276.6811251726610976, -45.00000000000000000 ) ) ;
#9614 = EDGE_CURVE ( 'NONE', #18134, #1534, #826, .T. ) ;
#9615 = CARTESIAN_POINT ( 'NONE',  ( 79.99999999999994316, 108.4677831376940560, -79.66646975086558768 ) ) ;
#9616 = CARTESIAN_POINT ( 'NONE',  ( -221.7152077904632677, 88.25158514949524147, -15.54860131211836993 ) ) ;
#9617 = CARTESIAN_POINT ( 'NONE',  ( 134.9999999999998579, 220.0000000000000284, 99.00000000000001421 ) ) ;
#9618 = DIRECTION ( 'NONE',  ( 0.000000000000000000, 0.000000000000000000, -1.000000000000000000 ) ) ;
#9619 = CARTESIAN_POINT ( 'NONE',  ( 33.10302365956999182, 203.2034914284457159, 15.00000000000000000 ) ) ;
#9620 = CARTESIAN_POINT ( 'NONE',  ( 176.5942101292460222, 101.9567147554491271, 45.00000000000000000 ) ) ;
#9621 = CIRCLE ( 'NONE', #6836, 22.49999999999999289 ) ;
#9622 = LINE ( 'NONE', #23255, #7868 ) ;
#9623 = EDGE_CURVE ( 'NONE', #15143, #4525, #16622, .T. ) ;
#9624 = CARTESIAN_POINT ( 'NONE',  ( 176.1454027868280434, 57.48855481560072889, 45.00000000000000000 ) ) ;
#9626 = ORIENTED_EDGE ( 'NONE', *, *, #15888, .T. ) ;
#9625 = ORIENTED_EDGE ( 'NONE', *, *, #7031, .F. ) ;
#9627 = PLANE ( 'NONE',  #5931 ) ;
#9628 = EDGE_CURVE ( 'NONE', #3224, #24423, #7030, .T. ) ;
#9629 = EDGE_CURVE ( 'NONE', #6895, #14227, #9595, .T. ) ;
#9630 = AXIS2_PLACEMENT_3D ( 'NONE', #21969, #17512, #15664 ) ;
#9631 = CARTESIAN_POINT ( 'NONE',  ( 90.00000000000024158, 240.0000000000000284, -6.270166537925966566 ) ) ;
#9632 = EDGE_CURVE ( 'NONE', #11042, #13747, #18358, .T. ) ;
#9633 = ORIENTED_EDGE ( 'NONE', *, *, #26461, .T. ) ;
#9635 = ORIENTED_EDGE ( 'NONE', *, *, #20310, .T. ) ;
#9634 = VECTOR ( 'NONE', #27285, 1000.000000000000000 ) ;
#9636 = DIRECTION ( 'NONE',  ( 0.000000000000000000, -0.000000000000000000, -1.000000000000000000 ) ) ;
#9637 = CARTESIAN_POINT ( 'NONE',  ( 157.4999999999998579, 201.1909374436971802, 45.00000000000000000 ) ) ;
#9638 = VERTEX_POINT ( 'NONE', #16895 ) ;
#9639 = VERTEX_POINT ( 'NONE', #15178 ) ;
#9640 = CARTESIAN_POINT ( 'NONE',  ( 134.9999999999998579, 220.0000000000000284, -169.9999999999999716 ) ) ;
#9641 = CARTESIAN_POINT ( 'NONE',  ( 157.4999999999998579, 83.32081209086616980, -45.00000000000000000 ) ) ;
#9642 = CIRCLE ( 'NONE', #17433, 5.999999999999991118 ) ;
#9643 = CARTESIAN_POINT ( 'NONE',  ( 158.0000000000002842, 178.8739998798873216, -45.00000000000000000 ) ) ;
#9644 = CARTESIAN_POINT ( 'NONE',  ( 91.50132543202619217, 230.4711603839584768, -17.28742811890413478 ) ) ;
#9645 = AXIS2_PLACEMENT_3D ( 'NONE', #27236, #3385, #16343 ) ;
#9646 = FACE_BOUND ( 'NONE', #10821, .T. ) ;
#9647 = CYLINDRICAL_SURFACE ( 'NONE', #11441, 9.999999999999994671 ) ;
#9648 = CARTESIAN_POINT ( 'NONE',  ( -213.2464434226970980, 57.29534669709769901, -37.98348409338405673 ) ) ;
#9649 = ADVANCED_FACE ( 'NONE', ( #19476 ), #6401, .T. ) ;
#9650 = ADVANCED_FACE ( 'NONE', ( #8279 ), #10434, .F. ) ;
#9651 = CARTESIAN_POINT ( 'NONE',  ( 157.4999999999997442, 256.3641876088515232, 45.00000000000000000 ) ) ;
#9652 = DIRECTION ( 'NONE',  ( -0.000000000000000000, 0.000000000000000000, 1.000000000000000000 ) ) ;
#9653 = CARTESIAN_POINT ( 'NONE',  ( 158.0000000000006253, 146.2716247822957598, 45.00000000000000000 ) ) ;
#9654 = LINE ( 'NONE', #5331, #17178 ) ;
#9655 = ORIENTED_EDGE ( 'NONE', *, *, #3785, .F. ) ;
#9656 = CARTESIAN_POINT ( 'NONE',  ( 157.4999999999998295, 226.2696875187675118, 45.00000000000000000 ) ) ;
#9657 = EDGE_CURVE ( 'NONE', #7774, #12951, #8424, .T. ) ;
#9658 = VECTOR ( 'NONE', #5956, 1000.000000000000114 ) ;
#9659 = EDGE_CURVE ( 'NONE', #26528, #1795, #27656, .T. ) ;
#9660 = FACE_OUTER_BOUND ( 'NONE', #22524, .T. ) ;
#9661 = LINE ( 'NONE', #25438, #23207 ) ;
#9662 = ORIENTED_EDGE ( 'NONE', *, *, #17251, .T. ) ;
#9663 = ORIENTED_EDGE ( 'NONE', *, *, #8884, .F. ) ;
#9664 = VECTOR ( 'NONE', #18176, 1000.000000000000000 ) ;
#9665 = CARTESIAN_POINT ( 'NONE',  ( 109.5756401952765486, 134.3783162856070703, 89.68749999971406339 ) ) ;
#9666 = DIRECTION ( 'NONE',  ( -0.8660254037844362651, 0.5000000000000039968, -0.000000000000000000 ) ) ;
#9667 = VERTEX_POINT ( 'NONE', #15032 ) ;
#9668 = ORIENTED_EDGE ( 'NONE', *, *, #28147, .F. ) ;
#9669 = CARTESIAN_POINT ( 'NONE',  ( -76.25760768171835480, 219.6666220619077876, 12.99999999999999822 ) ) ;
#9670 = FACE_OUTER_BOUND ( 'NONE', #6442, .T. ) ;
#9671 = DIRECTION ( 'NONE',  ( 1.000000000000000000, -0.000000000000000000, -0.000000000000000000 ) ) ;
#9672 = ORIENTED_EDGE ( 'NONE', *, *, #25535, .T. ) ;
#9673 = CARTESIAN_POINT ( 'NONE',  ( 158.0000000000000000, 206.4606249624626457, 45.00000000000000000 ) ) ;
#9674 = VERTEX_POINT ( 'NONE', #17035 ) ;
#9675 = LINE ( 'NONE', #22606, #24929 ) ;
#9676 = VECTOR ( 'NONE', #13754, 1000.000000000000000 ) ;
#9677 = CARTESIAN_POINT ( 'NONE',  ( -71.37541315349507443, 230.0000000000000000, -15.00000000000000000 ) ) ;
#9678 = CARTESIAN_POINT ( 'NONE',  ( 158.0000000000014211, 70.52749954957745615, 45.00000000000000000 ) ) ;
#9679 = CARTESIAN_POINT ( 'NONE',  ( 0.8309465671043746449, 136.6869851649963721, -15.12344959194870420 ) ) ;
#9680 = DIRECTION ( 'NONE',  ( 0.000000000000000000, 0.000000000000000000, -1.000000000000000000 ) ) ;
#9681 = CARTESIAN_POINT ( 'NONE',  ( -214.3828916364065833, 175.2783111443768576, 12.99999999999999822 ) ) ;
#9682 = CARTESIAN_POINT ( 'NONE',  ( 162.3518214533014543, 207.6748957395177229, -139.8013169873308073 ) ) ;
#9683 = EDGE_CURVE ( 'NONE', #14281, #3012, #18431, .T. ) ;
#9684 = EDGE_LOOP ( 'NONE', ( #15667, #20286 ) ) ;
#9685 = CARTESIAN_POINT ( 'NONE',  ( 187.4999999999996305, 288.9665627064425166, 45.00000000000000000 ) ) ;
#9686 = PLANE ( 'NONE',  #91 ) ;
#9687 = DIRECTION ( 'NONE',  ( 0.000000000000000000, 0.000000000000000000, -1.000000000000000000 ) ) ;
#9688 = ORIENTED_EDGE ( 'NONE', *, *, #16523, .F. ) ;
#9689 = LINE ( 'NONE', #5508, #2712 ) ;
#9690 = ORIENTED_EDGE ( 'NONE', *, *, #7994, .F. ) ;
#9691 = CARTESIAN_POINT ( 'NONE',  ( -189.8086322075389774, 92.49158130768422836, 15.00000000000000000 ) ) ;
#9692 = DIRECTION ( 'NONE',  ( 0.8314772792026894344, -0.5555587585212683477, 0.000000000000000000 ) ) ;
#9693 = CARTESIAN_POINT ( 'NONE',  ( -210.0000000000000568, -80.00000000000049738, 29.99999999999995737 ) ) ;
#9694 = ORIENTED_EDGE ( 'NONE', *, *, #11480, .F. ) ;
#9695 = LINE ( 'NONE', #22195, #13857 ) ;
#9696 =( NAMED_UNIT ( * ) PLANE_ANGLE_UNIT ( ) SI_UNIT ( $, .RADIAN. ) );
#9697 = VERTEX_POINT ( 'NONE', #8135 ) ;
#9698 = ADVANCED_FACE ( 'NONE', ( #19188 ), #25793, .T. ) ;
#9699 = VECTOR ( 'NONE', #24842, 1000.000000000000000 ) ;
#9700 = CARTESIAN_POINT ( 'NONE',  ( 502.4999999999996021, 494.4107529906318632, 75.35061095560301681 ) ) ;
#9701 = CARTESIAN_POINT ( 'NONE',  ( 99.17402272717502854, 242.2128782075101867, 12.79878931498954486 ) ) ;
#9702 = ORIENTED_EDGE ( 'NONE', *, *, #13189, .F. ) ;
#9703 = ORIENTED_EDGE ( 'NONE', *, *, #23058, .F. ) ;
#9704 = CARTESIAN_POINT ( 'NONE',  ( -160.0000000000000284, 119.7660240611718905, -22.85081902853004721 ) ) ;
#9705 = EDGE_LOOP ( 'NONE', ( #17071, #21972, #10371, #5507, #7445, #26213, #26647, #8840 ) ) ;
#9706 = CIRCLE ( 'NONE', #13376, 6.000000000000005329 ) ;
#9707 = EDGE_LOOP ( 'NONE', ( #10395, #6543, #8600, #17322 ) ) ;
#9708 = VERTEX_POINT ( 'NONE', #14897 ) ;
#9709 = EDGE_CURVE ( 'NONE', #8771, #23789, #4241, .T. ) ;
#9710 = CARTESIAN_POINT ( 'NONE',  ( 107.9865739111272944, 251.1735473298315355, 29.61538987307772430 ) ) ;
#9711 = EDGE_CURVE ( 'NONE', #3815, #4843, #1664, .T. ) ;
#9712 = LINE ( 'NONE', #20484, #25005 ) ;
#9713 = CARTESIAN_POINT ( 'NONE',  ( 158.0000000000001705, 190.9054999099155054, 45.00000000000000000 ) ) ;
#9714 = LINE ( 'NONE', #18054, #21575 ) ;
#9715 = LINE ( 'NONE', #27090, #21369 ) ;
#9716 = EDGE_CURVE ( 'NONE', #8492, #26679, #21628, .T. ) ;
#9717 = CARTESIAN_POINT ( 'NONE',  ( 158.0000000000000568, 203.4448749474510407, 45.00000000000000000 ) ) ;
#9718 = VECTOR ( 'NONE', #12449, 1000.000000000000000 ) ;
#9719 = LINE ( 'NONE', #9293, #22321 ) ;
#9720 = DIRECTION ( 'NONE',  ( 0.000000000000000000, 0.000000000000000000, 1.000000000000000000 ) ) ;
#9721 = CARTESIAN_POINT ( 'NONE',  ( -263.9041850570887959, -171.3165909455712494, 104.9297054525729322 ) ) ;
#9723 = DIRECTION ( 'NONE',  ( 0.000000000000000000, 0.7071067811865476838, 0.7071067811865474617 ) ) ;
#9722 = VECTOR ( 'NONE', #7920, 1000.000000000000114 ) ;
#9724 = FACE_OUTER_BOUND ( 'NONE', #8237, .T. ) ;
#9725 = CIRCLE ( 'NONE', #24392, 7.507013428474183847 ) ;
#9726 = VERTEX_POINT ( 'NONE', #21483 ) ;
#9727 = AXIS2_PLACEMENT_3D ( 'NONE', #27542, #18658, #5582 ) ;
#9728 = DIRECTION ( 'NONE',  ( -0.8916010070295922185, 0.4528218681378110011, 0.000000000000000000 ) ) ;
#9729 = DIRECTION ( 'NONE',  ( 0.8660254037844432595, 0.4999999999999918954, 0.000000000000000000 ) ) ;
#9730 = DIRECTION ( 'NONE',  ( 0.000000000000000000, -0.000000000000000000, -1.000000000000000000 ) ) ;
#9731 = ORIENTED_EDGE ( 'NONE', *, *, #18839, .F. ) ;
#9732 = EDGE_CURVE ( 'NONE', #14031, #10648, #1798, .T. ) ;
#9733 = ADVANCED_FACE ( 'NONE', ( #17180 ), #19331, .T. ) ;
#9734 = CARTESIAN_POINT ( 'NONE',  ( -210.0000000000000568, 0.000000000000000000, 110.0000000000000284 ) ) ;
#9735 = ORIENTED_EDGE ( 'NONE', *, *, #20496, .T. ) ;
#9736 = CARTESIAN_POINT ( 'NONE',  ( -305.0000000000001137, -157.0000000000000284, 60.00000000000002842 ) ) ;
#9737 = ORIENTED_EDGE ( 'NONE', *, *, #25783, .F. ) ;
#9738 = CIRCLE ( 'NONE', #20736, 10.00000000000000888 ) ;
#9739 = ORIENTED_EDGE ( 'NONE', *, *, #1216, .F. ) ;
#9740 = VERTEX_POINT ( 'NONE', #21201 ) ;
#9741 = ORIENTED_EDGE ( 'NONE', *, *, #15800, .T. ) ;
#9742 = VECTOR ( 'NONE', #11516, 1000.000000000000114 ) ;
#9743 = LINE ( 'NONE', #26836, #20974 ) ;
#9744 = EDGE_CURVE ( 'NONE', #12291, #21738, #19411, .T. ) ;
#9745 = CARTESIAN_POINT ( 'NONE',  ( 158.0000000000011369, 96.11412463215494029, 45.00000000000000000 ) ) ;
#9746 = CARTESIAN_POINT ( 'NONE',  ( -260.0000000000001137, -157.0000000000000284, 105.0000000000000142 ) ) ;
#9747 = CIRCLE ( 'NONE', #11109, 11.00000000000001066 ) ;
#9748 = FACE_OUTER_BOUND ( 'NONE', #27517, .T. ) ;
#9749 = UNCERTAINTY_MEASURE_WITH_UNIT (LENGTH_MEASURE( 1.000000000000000082E-05 ), #17558, 'distance_accuracy_value', 'NONE');
#9750 = EDGE_CURVE ( 'NONE', #8949, #14118, #4586, .T. ) ;
#9751 = PLANE ( 'NONE',  #24496 ) ;
#9752 = EDGE_CURVE ( 'NONE', #21276, #4661, #5630, .T. ) ;
#9753 = CARTESIAN_POINT ( 'NONE',  ( -214.1728591254723142, 55.16903133821974592, 44.30008786503535845 ) ) ;
#9754 = FACE_OUTER_BOUND ( 'NONE', #15532, .T. ) ;
#9755 = CARTESIAN_POINT ( 'NONE',  ( 65.00000000000000000, -150.0000000000000568, 70.00000000000001421 ) ) ;
#9756 = CARTESIAN_POINT ( 'NONE',  ( 157.9999999999998010, 241.0630000600560550, 45.00000000000000000 ) ) ;
#9757 = LINE ( 'NONE', #7600, #25470 ) ;
#9758 = EDGE_CURVE ( 'NONE', #3282, #6570, #22054, .T. ) ;
#9759 = CARTESIAN_POINT ( 'NONE',  ( 158.0000000000002274, 185.8897498949014278, 45.00000000000000000 ) ) ;
#9760 = CARTESIAN_POINT ( 'NONE',  ( -146.6428522700808230, 74.54464929955099706, 83.00000000000001421 ) ) ;
#9761 = CARTESIAN_POINT ( 'NONE',  ( 134.9999999999998579, 220.0000000000000284, 153.1081322850112940 ) ) ;
#9762 = AXIS2_PLACEMENT_3D ( 'NONE', #14448, #23062, #3371 ) ;
#9763 = CIRCLE ( 'NONE', #6525, 6.000000000000005329 ) ;
#9764 = CARTESIAN_POINT ( 'NONE',  ( 134.9999999999998863, 537.6859242279716682, -145.0000000000000000 ) ) ;
#9765 = CARTESIAN_POINT ( 'NONE',  ( 114.5273445118729541, 107.2595481030940761, -100.0000000000000142 ) ) ;
#9766 = CARTESIAN_POINT ( 'NONE',  ( 157.4999999999998579, 220.0000000000000284, -84.99999999999997158 ) ) ;
#9767 = VECTOR ( 'NONE', #19404, 1000.000000000000000 ) ;
#9769 = ORIENTED_EDGE ( 'NONE', *, *, #5841, .F. ) ;
#9768 = ORIENTED_EDGE ( 'NONE', *, *, #22693, .F. ) ;
#9770 = VECTOR ( 'NONE', #20396, 1000.000000000000000 ) ;
#9771 = LINE ( 'NONE', #18528, #12514 ) ;
#9772 = B_SPLINE_CURVE_WITH_KNOTS ( 'NONE', 3,
 ( #291, #7180, #2860, #9047, #26283, #15384, #17950, #6604, #15951, #24138, #22695, #11791, #1130, #24986, #23115, #7325, #5302, #1271, #22972, #2999, #27133, #25405 ),
 .UNSPECIFIED., .F., .F.,
 ( 4, 2, 2, 2, 2, 2, 2, 2, 2, 2, 4 ),
 ( 0.000000000000000000, 0.006670623320370424290, 0.01334124664074084858, 0.02001186996111127200, 0.02334718162129648458, 0.02668249328148169716, 0.03335311660185202171, 0.03668842826203719265, 0.04002373992222235666, 0.04669436324259268467, 0.05336498656296301268 ),
 .UNSPECIFIED. ) ;
#9773 = ORIENTED_EDGE ( 'NONE', *, *, #19865, .T. ) ;
#9774 = VERTEX_POINT ( 'NONE', #367 ) ;
#9775 = ORIENTED_EDGE ( 'NONE', *, *, #6970, .T. ) ;
#9776 = ORIENTED_EDGE ( 'NONE', *, *, #3052, .F. ) ;
#9777 = LINE ( 'NONE', #18535, #17020 ) ;
#9778 = TOROIDAL_SURFACE ( 'NONE', #7939, 55.86582179324592090, 2.000000000000000000 ) ;
#9779 = CARTESIAN_POINT ( 'NONE',  ( 157.9999999999996305, 286.2047501951820436, 45.00000000000000000 ) ) ;
#9780 = VECTOR ( 'NONE', #25121, 1000.000000000000000 ) ;
#9781 = CYLINDRICAL_SURFACE ( 'NONE', #24761, 5.000000000000000000 ) ;
#9782 = AXIS2_PLACEMENT_3D ( 'NONE', #4301, #17369, #10485 ) ;
#9783 = CARTESIAN_POINT ( 'NONE',  ( 167.4999999999996589, 494.4107529906318632, -84.99999999999995737 ) ) ;
#9784 = EDGE_CURVE ( 'NONE', #12221, #4097, #10861, .T. ) ;
#9785 = AXIS2_PLACEMENT_3D ( 'NONE', #20924, #2972, #20644 ) ;
#9786 = EDGE_CURVE ( 'NONE', #18620, #6585, #17740, .T. ) ;
#9787 = DIRECTION ( 'NONE',  ( 1.000000000000000000, -8.220356446306165096E-16, 0.000000000000000000 ) ) ;
#9788 = CARTESIAN_POINT ( 'NONE',  ( 79.99999999999992895, 110.0000000000000000, -100.0000000000000142 ) ) ;
#9789 = CARTESIAN_POINT ( 'NONE',  ( 124.9999999999998579, 220.0000000000000284, -99.00000000000001421 ) ) ;
#9790 = CARTESIAN_POINT ( 'NONE',  ( -210.1614673636062207, 73.84361952687928010, -34.09424755233946769 ) ) ;
#9791 = CARTESIAN_POINT ( 'NONE',  ( 109.2152537968686232, 204.6604904840920653, -138.9999999999999432 ) ) ;
#9792 = DIRECTION ( 'NONE',  ( -0.000000000000000000, -0.000000000000000000, -1.000000000000000000 ) ) ;
#9793 = DIRECTION ( 'NONE',  ( -0.000000000000000000, -0.000000000000000000, -1.000000000000000000 ) ) ;
#9794 = EDGE_LOOP ( 'NONE', ( #13265, #2660, #11041, #25973, #3166, #21702 ) ) ;
#9795 = VECTOR ( 'NONE', #7491, 1000.000000000000114 ) ;
#9796 = CARTESIAN_POINT ( 'NONE',  ( 5.999999999999998224, 0.000000000000000000, 0.000000000000000000 ) ) ;
#9797 = CIRCLE ( 'NONE', #25378, 6.000000000000005329 ) ;
#9798 = CARTESIAN_POINT ( 'NONE',  ( -228.6046226639666088, 73.96500373646588855, 16.69423931604977085 ) ) ;
#9799 = CARTESIAN_POINT ( 'NONE',  ( -36.37721155344281243, 172.2515494757248291, 45.00000000000000000 ) ) ;
#9800 = ORIENTED_EDGE ( 'NONE', *, *, #14950, .F. ) ;
#9801 = AXIS2_PLACEMENT_3D ( 'NONE', #14596, #18619, #18348 ) ;
#9802 = ORIENTED_EDGE ( 'NONE', *, *, #1014, .F. ) ;
#9803 = CARTESIAN_POINT ( 'NONE',  ( 100.5794065448834402, 118.1137289702941047, 99.99999999995674216 ) ) ;
#9804 = CARTESIAN_POINT ( 'NONE',  ( 157.9999999999999716, 208.9684999699701393, 45.00000000000000000 ) ) ;
#9805 = ORIENTED_EDGE ( 'NONE', *, *, #3407, .F. ) ;
#9806 = ORIENTED_EDGE ( 'NONE', *, *, #25316, .F. ) ;
#9807 = LINE ( 'NONE', #8208, #22815 ) ;
#9808 = CARTESIAN_POINT ( 'NONE',  ( 179.9999999999999147, -5.589247009368164321, 100.0000000000000142 ) ) ;
#9809 = CARTESIAN_POINT ( 'NONE',  ( 158.0000000000016200, 50.97237449702815582, -45.00000000000000000 ) ) ;
#9810 = VERTEX_POINT ( 'NONE', #11004 ) ;
#9811 = CARTESIAN_POINT ( 'NONE',  ( -260.0000000000001137, -220.0000000000000853, -59.99999999999986500 ) ) ;
#9812 = EDGE_LOOP ( 'NONE', ( #7523, #19041, #21817, #15429 ) ) ;
#9813 = CIRCLE ( 'NONE', #14889, 6.025000000000002132 ) ;
#9814 = CARTESIAN_POINT ( 'NONE',  ( -76.25760768171836901, 154.8982798170083299, -13.00000000000000000 ) ) ;
#9815 = EDGE_CURVE ( 'NONE', #8138, #22744, #2361, .T. ) ;
#9816 = EDGE_CURVE ( 'NONE', #21445, #4287, #26794, .T. ) ;
#9817 = PLANE ( 'NONE',  #4851 ) ;
#9818 = DIRECTION ( 'NONE',  ( 0.000000000000000000, -1.000000000000000000, 0.000000000000000000 ) ) ;
#9819 = DIRECTION ( 'NONE',  ( -2.775557561562887407E-16, -3.668437989309015303E-32, 1.000000000000000000 ) ) ;
#9820 = VECTOR ( 'NONE', #21615, 1000.000000000000000 ) ;
#9821 = CARTESIAN_POINT ( 'NONE',  ( -210.0000000000000284, 59.99999999999993605, 70.00000000000000000 ) ) ;
#9822 = CARTESIAN_POINT ( 'NONE',  ( 179.9999999999999147, -5.589247009368136787, -84.99999999999997158 ) ) ;
#9823 = CARTESIAN_POINT ( 'NONE',  ( 163.0358885901997326, 209.3211669751875377, -141.3391815462163379 ) ) ;
#9824 = ORIENTED_EDGE ( 'NONE', *, *, #2428, .F. ) ;
#9825 = DIRECTION ( 'NONE',  ( 1.321694076934710155E-16, -1.000000000000000000, 0.000000000000000000 ) ) ;
#9826 = CARTESIAN_POINT ( 'NONE',  ( -63.57415822541634043, 0.000000000000000000, 100.0000000000000000 ) ) ;
#9827 = CARTESIAN_POINT ( 'NONE',  ( 158.0000000000000000, 208.4606249624626457, 45.00000000000000000 ) ) ;
#9828 = ORIENTED_EDGE ( 'NONE', *, *, #12097, .T. ) ;
#9829 = CARTESIAN_POINT ( 'NONE',  ( 158.0000000000002558, 181.3818748873943889, -45.00000000000000000 ) ) ;
#9830 = VERTEX_POINT ( 'NONE', #13169 ) ;
#9831 = DIRECTION ( 'NONE',  ( 0.000000000000000000, 0.000000000000000000, 1.000000000000000000 ) ) ;
#9832 = DIRECTION ( 'NONE',  ( 0.5555587585212683477, 0.8314772792026894344, 0.000000000000000000 ) ) ;
#9833 = DIRECTION ( 'NONE',  ( -0.000000000000000000, -1.000000000000000000, -0.000000000000000000 ) ) ;
#9834 = ORIENTED_EDGE ( 'NONE', *, *, #3310, .F. ) ;
#9835 = CARTESIAN_POINT ( 'NONE',  ( 157.9999999999997442, 256.1102501050980322, 45.00000000000000000 ) ) ;
#9836 = CARTESIAN_POINT ( 'NONE',  ( -210.0000000000000284, 59.99999999999993605, 100.0000000000000142 ) ) ;
#9837 = ORIENTED_EDGE ( 'NONE', *, *, #6764, .T. ) ;
#9838 = VECTOR ( 'NONE', #5424, 1000.000000000000227 ) ;
#9839 = CARTESIAN_POINT ( 'NONE',  ( -112.5534411697180559, 133.0508595578523909, 15.80357080798902913 ) ) ;
#9840 = CARTESIAN_POINT ( 'NONE',  ( 158.0000000000003979, 170.8424998498591663, -45.00000000000000000 ) ) ;
#9841 = ORIENTED_EDGE ( 'NONE', *, *, #12034, .F. ) ;
#9842 = AXIS2_PLACEMENT_3D ( 'NONE', #11683, #7636, #21375 ) ;
#9843 = ORIENTED_EDGE ( 'NONE', *, *, #13947, .F. ) ;
#9844 = PLANE ( 'NONE',  #20035 ) ;
#9845 = ORIENTED_EDGE ( 'NONE', *, *, #21025, .T. ) ;
#9846 = EDGE_CURVE ( 'NONE', #10091, #20874, #26489, .T. ) ;
#9847 = ORIENTED_EDGE ( 'NONE', *, *, #6896, .F. ) ;
#9848 = ORIENTED_EDGE ( 'NONE', *, *, #21293, .F. ) ;
#9849 = DIRECTION ( 'NONE',  ( -1.000000000000000000, 2.696301922142074142E-31, -2.220446049250266932E-15 ) ) ;
#9850 = EDGE_CURVE ( 'NONE', #3329, #21558, #11292, .T. ) ;
#9851 = LINE ( 'NONE', #18049, #25910 ) ;
#9852 = CARTESIAN_POINT ( 'NONE',  ( -216.4421519707229891, 141.6000904446840707, -15.00000000000000000 ) ) ;
#9853 = AXIS2_PLACEMENT_3D ( 'NONE', #8506, #12406, #6339 ) ;
#9854 = DIRECTION ( 'NONE',  ( 0.000000000000000000, 1.000000000000000000, -1.224646799147353207E-16 ) ) ;
#9855 = PLANE ( 'NONE',  #8518 ) ;
#9856 = CARTESIAN_POINT ( 'NONE',  ( -261.1919288306253293, -171.9377729149742038, 95.00000000000004263 ) ) ;
#9857 = ADVANCED_FACE ( 'NONE', ( #4945 ), #6963, .F. ) ;
#9858 = CARTESIAN_POINT ( 'NONE',  ( -219.2467648448761395, 139.5102435001769265, -15.00000000000000000 ) ) ;
#9859 = AXIS2_PLACEMENT_3D ( 'NONE', #23926, #14893, #23781 ) ;
#9860 = DIRECTION ( 'NONE',  ( 0.000000000000000000, -1.000000000000000000, 0.000000000000000000 ) ) ;
#9861 = DIRECTION ( 'NONE',  ( 0.8916010070299883461, 0.4528218681370311249, 0.000000000000000000 ) ) ;
#9862 = CARTESIAN_POINT ( 'NONE',  ( 217.4999999999996305, 44.41075299063186321, -100.0000000000000142 ) ) ;
#9863 = VERTEX_POINT ( 'NONE', #19615 ) ;
#9864 = FACE_OUTER_BOUND ( 'NONE', #18627, .T. ) ;
#9865 = DIRECTION ( 'NONE',  ( -0.000000000000000000, -0.000000000000000000, -1.000000000000000000 ) ) ;
#9866 = DIRECTION ( 'NONE',  ( 0.8018642810807398158, 0.5975062131282554700, -0.000000000000000000 ) ) ;
#9867 = FACE_BOUND ( 'NONE', #1974, .T. ) ;
#9868 = VERTEX_POINT ( 'NONE', #28353 ) ;
#9869 = ADVANCED_FACE ( 'NONE', ( #17456 ), #20891, .F. ) ;
#9870 = DIRECTION ( 'NONE',  ( -0.000000000000000000, 0.000000000000000000, -1.000000000000000000 ) ) ;
#9871 = ORIENTED_EDGE ( 'NONE', *, *, #1149, .F. ) ;
#9872 = SURFACE_SIDE_STYLE ('',( #16071 ) ) ;
#9873 = EDGE_LOOP ( 'NONE', ( #26417, #663, #26290, #11138 ) ) ;
#9874 = CIRCLE ( 'NONE', #23176, 7.999999999999979572 ) ;
#9875 = AXIS2_PLACEMENT_3D ( 'NONE', #603, #2887, #9508 ) ;
#9876 = ORIENTED_EDGE ( 'NONE', *, *, #24404, .T. ) ;
#9877 = EDGE_CURVE ( 'NONE', #14406, #23088, #26936, .T. ) ;
#9878 = ORIENTED_EDGE ( 'NONE', *, *, #9337, .F. ) ;
#9879 = ORIENTED_EDGE ( 'NONE', *, *, #8445, .T. ) ;
#9880 = VECTOR ( 'NONE', #10820, 1000.000000000000000 ) ;
#9881 = ORIENTED_EDGE ( 'NONE', *, *, #21508, .F. ) ;
#9882 = CARTESIAN_POINT ( 'NONE',  ( 157.9999999999996305, 283.6968751876750616, 45.00000000000000000 ) ) ;
#9883 = CARTESIAN_POINT ( 'NONE',  ( 89.99999999999994316, -90.00000000000001421, -70.00000000000001421 ) ) ;
#9884 = DIRECTION ( 'NONE',  ( -0.8916010070293584056, 0.4528218681382713551, 0.000000000000000000 ) ) ;
#9885 = ADVANCED_BREP_SHAPE_REPRESENTATION ( '', ( #27732, #10637 ), #6979 ) ;
#9886 = CARTESIAN_POINT ( 'NONE',  ( -77.52803642472932211, 136.3040012171963156, -13.50820732054850559 ) ) ;
#9887 = FACE_OUTER_BOUND ( 'NONE', #14819, .T. ) ;
#9888 = CARTESIAN_POINT ( 'NONE',  ( 157.4999999999998579, 50.71843699327460797, 45.00000000000000000 ) ) ;
#9889 = CARTESIAN_POINT ( 'NONE',  ( 122.8247714198253959, 235.8670668058242939, -45.00000000000000000 ) ) ;
#9890 = CARTESIAN_POINT ( 'NONE',  ( -90.19911340583169590, 136.4341784506709416, -13.48770749977458294 ) ) ;
#9891 = ADVANCED_FACE ( 'NONE', ( #24926 ), #16175, .T. ) ;
#9892 = ADVANCED_FACE ( 'NONE', ( #796 ), #3075, .F. ) ;
#9893 = DIRECTION ( 'NONE',  ( 0.8916010070293584056, -0.4528218681382712996, 0.000000000000000000 ) ) ;
#9894 = AXIS2_PLACEMENT_3D ( 'NONE', #6516, #15012, #12860 ) ;
#9895 = CARTESIAN_POINT ( 'NONE',  ( -208.4641541919228871, 89.68079096126031402, -24.78256666906890260 ) ) ;
#9896 = FILL_AREA_STYLE ('',( #3552 ) ) ;
#9897 = DIRECTION ( 'NONE',  ( 1.000000000000000000, 0.000000000000000000, 0.000000000000000000 ) ) ;
#9898 = AXIS2_PLACEMENT_3D ( 'NONE', #13424, #11273, #2484 ) ;
#9899 = FACE_OUTER_BOUND ( 'NONE', #11909, .T. ) ;
#9900 = AXIS2_PLACEMENT_3D ( 'NONE', #13614, #26658, #680 ) ;
#9901 = ORIENTED_EDGE ( 'NONE', *, *, #16934, .T. ) ;
#9902 = FACE_OUTER_BOUND ( 'NONE', #21917, .T. ) ;
#9903 = CARTESIAN_POINT ( 'NONE',  ( 65.00000000000000000, -150.0000000000000568, -69.99999999999998579 ) ) ;
#9904 = DIRECTION ( 'NONE',  ( -0.000000000000000000, -0.000000000000000000, 1.000000000000000000 ) ) ;
#9905 = AXIS2_PLACEMENT_3D ( 'NONE', #12523, #16823, #25713 ) ;
#9907 = ORIENTED_EDGE ( 'NONE', *, *, #21024, .F. ) ;
#9906 = ORIENTED_EDGE ( 'NONE', *, *, #20620, .F. ) ;
#9908 = EDGE_CURVE ( 'NONE', #11767, #12751, #18734, .T. ) ;
#9909 = EDGE_CURVE ( 'NONE', #5308, #10360, #22486, .T. ) ;
#9910 = DIRECTION ( 'NONE',  ( -0.000000000000000000, -1.000000000000000000, -0.000000000000000000 ) ) ;
#9911 = ORIENTED_EDGE ( 'NONE', *, *, #19623, .F. ) ;
#9912 = ORIENTED_EDGE ( 'NONE', *, *, #11402, .F. ) ;
#9913 = ORIENTED_EDGE ( 'NONE', *, *, #1452, .F. ) ;
#9914 = ORIENTED_EDGE ( 'NONE', *, *, #7705, .F. ) ;
#9915 = AXIS2_PLACEMENT_3D ( 'NONE', #2135, #13646, #8896 ) ;
#9916 = ADVANCED_FACE ( 'NONE', ( #656 ), #16316, .T. ) ;
#9917 = EDGE_LOOP ( 'NONE', ( #3313, #5200, #10711, #4137 ) ) ;
#9918 = LINE ( 'NONE', #22711, #5252 ) ;
#9919 = VECTOR ( 'NONE', #7962, 1000.000000000000000 ) ;
#9920 = DIRECTION ( 'NONE',  ( 1.000000000000000000, 0.000000000000000000, 0.000000000000000000 ) ) ;
#9921 = CARTESIAN_POINT ( 'NONE',  ( 158.0000000000015064, 61.00387452705632541, -45.00000000000000000 ) ) ;
#9922 = CARTESIAN_POINT ( 'NONE',  ( 101.6154897312858338, 236.6169605195232748, -24.18002435645406933 ) ) ;
#9923 = CARTESIAN_POINT ( 'NONE',  ( -4.730967070951327180, 132.3085785638695029, -15.99979783535312983 ) ) ;
#9924 = CARTESIAN_POINT ( 'NONE',  ( -112.3221550338875687, 69.54464929955099706, 83.00000000000001421 ) ) ;
#9925 = DIRECTION ( 'NONE',  ( 0.8916010070299672519, -0.4528218681370723142, 0.000000000000000000 ) ) ;
#9926 = DIRECTION ( 'NONE',  ( -0.000000000000000000, 0.000000000000000000, 1.000000000000000000 ) ) ;
#9927 = LINE ( 'NONE', #18820, #11885 ) ;
#9928 = FACE_OUTER_BOUND ( 'NONE', #15753, .T. ) ;
#9929 = DIRECTION ( 'NONE',  ( -0.8916010070293283185, -0.4528218681383305855, 0.000000000000000000 ) ) ;
#9930 = CARTESIAN_POINT ( 'NONE',  ( 158.0000000000016485, 48.46449948952110987, 45.00000000000000000 ) ) ;
#9931 = VERTEX_POINT ( 'NONE', #2796 ) ;
#9932 = CIRCLE ( 'NONE', #13145, 5.000000000000004441 ) ;
#9933 = DIRECTION ( 'NONE',  ( -0.000000000000000000, -0.000000000000000000, -1.000000000000000000 ) ) ;
#9934 = DIRECTION ( 'NONE',  ( 0.2759800118297804916, -0.9611633748070274041, 0.000000000000000000 ) ) ;
#9935 = ORIENTED_EDGE ( 'NONE', *, *, #10766, .F. ) ;
#9936 = CARTESIAN_POINT ( 'NONE',  ( 0.000000000000000000, 0.000000000000000000, 0.000000000000000000 ) ) ;
#9937 = AXIS2_PLACEMENT_3D ( 'NONE', #16054, #25084, #5399 ) ;
#9938 = ORIENTED_EDGE ( 'NONE', *, *, #19617, .F. ) ;
#9940 = EDGE_CURVE ( 'NONE', #11012, #1342, #28043, .T. ) ;
#9939 = ORIENTED_EDGE ( 'NONE', *, *, #27561, .T. ) ;
#9941 = CARTESIAN_POINT ( 'NONE',  ( 157.4999999999998579, 88.33656210588026170, 45.00000000000000000 ) ) ;
#9942 = DIRECTION ( 'NONE',  ( 0.000000000000000000, 0.000000000000000000, 1.000000000000000000 ) ) ;
#9943 = ORIENTED_EDGE ( 'NONE', *, *, #111, .F. ) ;
#9944 = ORIENTED_EDGE ( 'NONE', *, *, #7790, .F. ) ;
#9945 = CARTESIAN_POINT ( 'NONE',  ( 79.99999999999991473, 110.0000000000000142, -70.00000000000001421 ) ) ;
#9946 = CARTESIAN_POINT ( 'NONE',  ( 93.83231682052215206, 231.2056562043867984, 18.37428548869055334 ) ) ;
#9947 = CARTESIAN_POINT ( 'NONE',  ( -210.0000000000000853, -218.4793454996984394, -90.61920026979450427 ) ) ;
#9948 = ORIENTED_EDGE ( 'NONE', *, *, #16340, .T. ) ;
#9949 = CARTESIAN_POINT ( 'NONE',  ( -229.6754219177769301, 91.64948492225875043, 13.10942810910360912 ) ) ;
#9950 = VERTEX_POINT ( 'NONE', #2944 ) ;
#9951 = TOROIDAL_SURFACE ( 'NONE', #3522, 421.5408555545579929, 7.500000000000000000 ) ;
#9952 = CARTESIAN_POINT ( 'NONE',  ( 1.982541115402066017E-14, -150.0000000000000568, 100.0000000000000142 ) ) ;
#9953 = FACE_OUTER_BOUND ( 'NONE', #18864, .T. ) ;
#9954 = CARTESIAN_POINT ( 'NONE',  ( -260.0000000000001137, -152.0000000000000284, -94.99999999999987210 ) ) ;
#9955 = DIRECTION ( 'NONE',  ( -0.6681556583950251094, -0.7440215159218921404, 0.000000000000000000 ) ) ;
#9956 = CARTESIAN_POINT ( 'NONE',  ( 9.999999999999964473, 60.00000000000001421, 100.0000000000000142 ) ) ;
#9957 = CARTESIAN_POINT ( 'NONE',  ( 157.4999999999998579, 221.2539375037535194, -45.00000000000000000 ) ) ;
#9958 = CARTESIAN_POINT ( 'NONE',  ( 161.9784637521712227, 206.8776822256648984, -150.6145052419836077 ) ) ;
#9959 = ORIENTED_EDGE ( 'NONE', *, *, #2759, .T. ) ;
#9960 = EDGE_CURVE ( 'NONE', #5589, #18109, #24390, .T. ) ;
#9961 = DIRECTION ( 'NONE',  ( 0.000000000000000000, 0.000000000000000000, -1.000000000000000000 ) ) ;
#9962 = CARTESIAN_POINT ( 'NONE',  ( -141.6428522700808230, 74.54464929955099706, 80.00000000000001421 ) ) ;
#9963 = DIRECTION ( 'NONE',  ( 0.8916010070295614653, -0.4528218681378716193, 0.000000000000000000 ) ) ;
#9964 = PLANE ( 'NONE',  #17604 ) ;
#9965 = ORIENTED_EDGE ( 'NONE', *, *, #4707, .F. ) ;
#9966 = CARTESIAN_POINT ( 'NONE',  ( 167.4999999999996589, 494.4107529906318632, 84.99999999999995737 ) ) ;
#9967 = ORIENTED_EDGE ( 'NONE', *, *, #8991, .T. ) ;
#9968 = CARTESIAN_POINT ( 'NONE',  ( 158.0000000000014211, 71.03537455708449500, 45.00000000000000000 ) ) ;
#9969 = CARTESIAN_POINT ( 'NONE',  ( 157.9999999999997726, 246.5866250825770294, 45.00000000000000000 ) ) ;
#9970 = FACE_OUTER_BOUND ( 'NONE', #16350, .T. ) ;
#9971 = VERTEX_POINT ( 'NONE', #7821 ) ;
#9972 = CARTESIAN_POINT ( 'NONE',  ( 0.3651377029009472697, 0.000000000000000000, 0.000000000000000000 ) ) ;
#9973 = CARTESIAN_POINT ( 'NONE',  ( -214.3828916364065833, 175.2783111443768576, 12.99999999999999822 ) ) ;
#9974 = EDGE_CURVE ( 'NONE', #11698, #2950, #11729, .T. ) ;
#9975 = EDGE_LOOP ( 'NONE', ( #15035, #14572, #18669, #1161 ) ) ;
#9976 = AXIS2_PLACEMENT_3D ( 'NONE', #13527, #593, #9359 ) ;
#9977 = EDGE_CURVE ( 'NONE', #11698, #3367, #16450, .T. ) ;
#9979 = EDGE_CURVE ( 'NONE', #18699, #22168, #22101, .T. ) ;
#9978 = CLOSED_SHELL ( 'NONE', ( #17937, #4050, #22931, #20228, #12190, #8509, #15540, #6627, #22494, #285, #9013, #24267, #3043, #20483, #8414, #9176, #8514, #23375, #4547, #6599, #987, #11583, #23139, #4947, #3760, #15991, #1107, #13447, #10050, #26765, #22461, #11078, #337, #14552, #14911, #8901, #27154, #9857, #15585, #10765, #5948, #1745, #702, #2298, #19718, #9495, #26359, #21373, #17581, #6417, #227, #15520, #12453, #7798, #12701, #7381, #13819, #24647, #5905, #27985, #8902, #1249, #13968, #26687, #25756, #27054, #1678, #1501, #22228, #6630, #4331, #21732, #15108, #13319, #18251, #937, #1045, #22388, #7513, #1275, #14798, #13015, #3563, #26691, #10788, #10686, #21776, #4128, #5421, #11453, #10730, #21407, #5874, #2879, #6784, #20831, #16067, #19048, #132, #12123, #5680, #17432, #14383, #24590, #4188, #14717, #17047, #5310, #12347, #22553, #21463, #19985, #15231, #23072, #4927, #18630, #26116, #23663, #17100, #22818, #443, #27380, #26367, #23694, #20867, #5529, #2854, #10486, #26594, #9064, #6169, #7119, #23252, #10776, #5573, #18689, #9892, #10632, #21656, #19669, #7776, #22822, #9916, #8620, #17514, #27344, #12930, #25317, #10389, #4148, #11131, #10966, #14467, #14437, #17327, #15682, #24723, #9399, #21064, #10720, #15095, #21223, #17003, #20766, #21870, #4749, #8256, #9, #7320, #5067, #6858, #4896, #16386, #7710, #13394, #26380, #14206, #20690, #1219, #14052, #25211, #1504, #5102, #15958, #14963, #25687, #14428, #16924, #20040, #27684, #20028, #24360, #11448, #22067, #18129, #310, #27260, #16594, #5656, #10852, #19716, #14506, #13283, #19822, #15952, #19905, #1143, #14638, #21187, #20241, #8476, #12786, #23851, #26332, #960, #20701, #19301, #2239, #10688, #14971, #22292, #10459, #18487, #21667, #27466, #22855, #3765, #17963, #6750, #673, #16641, #13312, #21027, #7269, #13223, #28256, #3370, #25242, #5557, #9649, #23664, #2967, #26429, #13168, #6523, #1046, #14712, #27261, #9733, #10589, #2761, #20691, #23013, #19881, #11342 ) ) ;
#9980 = DIRECTION ( 'NONE',  ( 0.000000000000000000, 0.000000000000000000, 1.000000000000000000 ) ) ;
#9981 = ADVANCED_FACE ( 'NONE', ( #26040 ), #7961, .F. ) ;
#9982 = CARTESIAN_POINT ( 'NONE',  ( 109.9934396465123001, 259.4709655040182383, 44.08366846580944554 ) ) ;
#9983 = ORIENTED_EDGE ( 'NONE', *, *, #16942, .F. ) ;
#9984 = ORIENTED_EDGE ( 'NONE', *, *, #19704, .F. ) ;
#9985 = DIRECTION ( 'NONE',  ( 1.000000000000000000, -0.000000000000000000, -0.000000000000000000 ) ) ;
#9986 = EDGE_LOOP ( 'NONE', ( #9361, #16922, #18318, #18180 ) ) ;
#9987 = ORIENTED_EDGE ( 'NONE', *, *, #25002, .F. ) ;
#9988 = ORIENTED_EDGE ( 'NONE', *, *, #19694, .F. ) ;
#9989 = PLANE ( 'NONE',  #18469 ) ;
#9990 = VECTOR ( 'NONE', #26916, 1000.000000000000000 ) ;
#9991 = CARTESIAN_POINT ( 'NONE',  ( -221.3650667873343139, -91.18033988749901653, 0.000000000000000000 ) ) ;
#9992 = LINE ( 'NONE', #23065, #24306 ) ;
#9993 = AXIS2_PLACEMENT_3D ( 'NONE', #26535, #20224, #556 ) ;
#9994 = AXIS2_PLACEMENT_3D ( 'NONE', #15334, #26501, #22602 ) ;
#9995 = CARTESIAN_POINT ( 'NONE',  ( 116.8899838958981974, 206.6356889813898192, -99.51050955275447052 ) ) ;
#9996 = CARTESIAN_POINT ( 'NONE',  ( 134.9999999999998579, 220.0000000000000284, -119.9999999999999858 ) ) ;
#9997 = CARTESIAN_POINT ( 'NONE',  ( 134.9999999999998579, -327.2004514666934369, 84.99999999999995737 ) ) ;
#9998 = CARTESIAN_POINT ( 'NONE',  ( -205.7061355896894383, 146.0477147645469813, 15.00000000000000000 ) ) ;
#9999 = CARTESIAN_POINT ( 'NONE',  ( -277.2150368962633706, -170.0000000000001421, 101.5769467933889558 ) ) ;
#10000 = CARTESIAN_POINT ( 'NONE',  ( 0.000000000000000000, 0.000000000000000000, 0.000000000000000000 ) ) ;
#10001 = CARTESIAN_POINT ( 'NONE',  ( 128.0812361363530272, 198.0425250404537394, 45.00000000000000000 ) ) ;
#10002 = ORIENTED_EDGE ( 'NONE', *, *, #1996, .F. ) ;
#10003 = CARTESIAN_POINT ( 'NONE',  ( -20.30805539402063431, 129.6344908925467223, 15.47809640394222086 ) ) ;
#10004 = EDGE_CURVE ( 'NONE', #3340, #14776, #4058, .T. ) ;
#10005 = EDGE_CURVE ( 'NONE', #17429, #26528, #10540, .T. ) ;
#10006 = CARTESIAN_POINT ( 'NONE',  ( 100.4596362579077464, 242.9371632374793819, -14.31520527065961979 ) ) ;
#10007 = DIRECTION ( 'NONE',  ( 0.8916010070295922185, 0.4528218681378110011, 0.000000000000000000 ) ) ;
#10008 = FACE_OUTER_BOUND ( 'NONE', #11130, .T. ) ;
#10009 = CARTESIAN_POINT ( 'NONE',  ( -217.2892621185082760, 109.4029876883478352, -13.00000000000000000 ) ) ;
#10010 = ORIENTED_EDGE ( 'NONE', *, *, #21676, .T. ) ;
#10011 = AXIS2_PLACEMENT_3D ( 'NONE', #1265, #14215, #23384 ) ;
#10012 = DIRECTION ( 'NONE',  ( 0.8916010070297338830, -0.4528218681375318910, 0.000000000000000000 ) ) ;
#10013 = ORIENTED_EDGE ( 'NONE', *, *, #10296, .T. ) ;
#10014 = EDGE_CURVE ( 'NONE', #25748, #12291, #12568, .T. ) ;
#10015 = DIRECTION ( 'NONE',  ( 0.8379557447115549840, 0.5457381880580680633, 0.000000000000000000 ) ) ;
#10016 = VECTOR ( 'NONE', #17299, 1000.000000000000000 ) ;
#10017 = VERTEX_POINT ( 'NONE', #17143 ) ;
#10018 = VERTEX_POINT ( 'NONE', #19155 ) ;
#10019 = EDGE_CURVE ( 'NONE', #12783, #27491, #12710, .T. ) ;
#10020 = APPLICATION_CONTEXT ( 'automotive_design' ) ;
#10021 = ORIENTED_EDGE ( 'NONE', *, *, #585, .T. ) ;
#10022 = ORIENTED_EDGE ( 'NONE', *, *, #3698, .T. ) ;
#10023 = CARTESIAN_POINT ( 'NONE',  ( 151.9705627484771355, 204.4436508138959141, -45.00000000000000000 ) ) ;
#10024 = CARTESIAN_POINT ( 'NONE',  ( 157.4999999999998579, 135.9861872485140850, 45.00000000000000000 ) ) ;
#10025 = CARTESIAN_POINT ( 'NONE',  ( -210.0000000000000568, -220.0000000000000853, -90.87829376371895762 ) ) ;
#10026 = AXIS2_PLACEMENT_3D ( 'NONE', #15068, #1980, #10757 ) ;
#10027 = CARTESIAN_POINT ( 'NONE',  ( -160.8326600028555617, 120.2355194873574931, -21.37420696376538132 ) ) ;
#10028 = CARTESIAN_POINT ( 'NONE',  ( -214.3828916364065833, 175.2783111443768576, 15.00000000000000000 ) ) ;
#10030 = CARTESIAN_POINT ( 'NONE',  ( 158.0000000000004832, 163.3188748273380213, 45.00000000000000000 ) ) ;
#10029 = TOROIDAL_SURFACE ( 'NONE', #17359, 55.86582179324592090, 2.000000000000000000 ) ;
#10031 = CARTESIAN_POINT ( 'NONE',  ( -135.1351637729545700, 129.7127537419684700, -15.41371473069906095 ) ) ;
#10032 = CARTESIAN_POINT ( 'NONE',  ( 158.0000000000007390, 135.7322497447605656, 45.00000000000000000 ) ) ;
#10033 = VECTOR ( 'NONE', #18160, 1000.000000000000227 ) ;
#10034 = CARTESIAN_POINT ( 'NONE',  ( -175.0000000000000000, -120.0000000000001705, 64.00000000000002842 ) ) ;
#10035 =( LENGTH_UNIT ( ) NAMED_UNIT ( * ) SI_UNIT ( .MILLI., .METRE. ) );
#10036 = DIRECTION ( 'NONE',  ( 1.000000000000000000, 0.000000000000000000, 0.000000000000000000 ) ) ;
#10037 = LINE ( 'NONE', #14495, #8383 ) ;
#10038 = EDGE_LOOP ( 'NONE', ( #17107, #8396, #7157, #17582 ) ) ;
#10039 = EDGE_CURVE ( 'NONE', #4814, #24608, #1491, .T. ) ;
#10040 = DIRECTION ( 'NONE',  ( 0.000000000000000000, -2.498359269027536321E-16, 1.000000000000000000 ) ) ;
#10041 = CARTESIAN_POINT ( 'NONE',  ( 65.00000000000000000, -120.0000000000000995, -75.99999999999998579 ) ) ;
#10043 = ORIENTED_EDGE ( 'NONE', *, *, #11291, .F. ) ;
#10042 = ORIENTED_EDGE ( 'NONE', *, *, #6337, .T. ) ;
#10044 = VECTOR ( 'NONE', #27925, 1000.000000000000000 ) ;
#10045 = CARTESIAN_POINT ( 'NONE',  ( 179.9999999999999147, 526.4263741777961059, -84.99999999999997158 ) ) ;
#10046 = EDGE_LOOP ( 'NONE', ( #25832, #145, #17536, #8367 ) ) ;
#10047 = ORIENTED_EDGE ( 'NONE', *, *, #5128, .F. ) ;
#10048 = ORIENTED_EDGE ( 'NONE', *, *, #13485, .T. ) ;
#10049 = VECTOR ( 'NONE', #15450, 1000.000000000000000 ) ;
#10050 = ADVANCED_FACE ( 'NONE', ( #19019 ), #19296, .F. ) ;
#10051 = EDGE_CURVE ( 'NONE', #26218, #26681, #12025, .T. ) ;
#10052 = AXIS2_PLACEMENT_3D ( 'NONE', #9956, #21429, #23731 ) ;
#10053 = ORIENTED_EDGE ( 'NONE', *, *, #19705, .T. ) ;
#10054 = ORIENTED_EDGE ( 'NONE', *, *, #26503, .F. ) ;
#10055 = EDGE_LOOP ( 'NONE', ( #20715, #16848, #11184, #27883, #3396, #9731, #7586, #24652 ) ) ;
#10056 = PLANE ( 'NONE',  #7207 ) ;
#10057 = VECTOR ( 'NONE', #452, 1000.000000000000000 ) ;
#10058 = DIRECTION ( 'NONE',  ( 1.000000000000000000, 0.000000000000000000, 0.000000000000000000 ) ) ;
#10059 = PLANE ( 'NONE',  #11658 ) ;
#10060 = EDGE_CURVE ( 'NONE', #23339, #25239, #14716, .T. ) ;
#10061 = CARTESIAN_POINT ( 'NONE',  ( 157.4999999999998579, 186.1436873986549188, -45.00000000000000000 ) ) ;
#10062 = EDGE_CURVE ( 'NONE', #27410, #21564, #5802, .T. ) ;
#10063 = VECTOR ( 'NONE', #7250, 1000.000000000000000 ) ;
#10064 = DIRECTION ( 'NONE',  ( 0.000000000000000000, 0.000000000000000000, 1.000000000000000000 ) ) ;
#10065 = B_SPLINE_CURVE_WITH_KNOTS ( 'NONE', 3,
 ( #11643, #14214, #16091, #27263, #13648, #7172, #848, #9895, #22964, #15946, #5294, #24696, #2708, #3267, #18651, #12059, #24551, #14077, #9616, #5003, #4860, #9479, #22828, #13796, #11496, #20662, #566, #16368, #9331, #22543 ),
 .UNSPECIFIED., .F., .F.,
 ( 4, 2, 2, 2, 2, 2, 2, 2, 2, 2, 2, 2, 2, 2, 4 ),
 ( 3.469446951953614189E-18, 0.002229328859797958130, 0.004458657719595912790, 0.006687986579393867884, 0.008917315439191822110, 0.01337597315878773230, 0.01783463087838364075, 0.02006395973818160192, 0.02229328859797955961, 0.02452261745777752078, 0.02675194631757547847, 0.03121060403717131754, 0.03232526846707026169, 0.03343993289696921278, 0.03566926175676703170 ),
 .UNSPECIFIED. ) ;
#10066 = CARTESIAN_POINT ( 'NONE',  ( 158.0000000000000853, 198.9369999399436892, 45.00000000000000000 ) ) ;
#10067 = LINE ( 'NONE', #19104, #10680 ) ;
#10068 = VECTOR ( 'NONE', #11353, 1000.000000000000114 ) ;
#10069 = CARTESIAN_POINT ( 'NONE',  ( 9.345921402568846403, 139.9999999999999716, -15.00000000000000000 ) ) ;
#10070 = DIRECTION ( 'NONE',  ( 0.000000000000000000, 0.000000000000000000, 1.000000000000000000 ) ) ;
#10071 = DIRECTION ( 'NONE',  ( 0.7071067811865474617, 0.000000000000000000, -0.7071067811865474617 ) ) ;
#10072 = EDGE_LOOP ( 'NONE', ( #26358, #11768, #25724, #15397 ) ) ;
#10073 = CARTESIAN_POINT ( 'NONE',  ( -203.2481855153402250, 92.57460631283321106, 29.78692811926997308 ) ) ;
#10074 = AXIS2_PLACEMENT_3D ( 'NONE', #21393, #25552, #1843 ) ;
#10075 = LINE ( 'NONE', #11960, #5304 ) ;
#10076 = ORIENTED_EDGE ( 'NONE', *, *, #9632, .F. ) ;
#10077 = PRODUCT_CONTEXT ( 'NONE', #12422, 'mechanical' ) ;
#10078 = ORIENTED_EDGE ( 'NONE', *, *, #16975, .T. ) ;
#10079 = ORIENTED_EDGE ( 'NONE', *, *, #1360, .F. ) ;
#10080 = EDGE_CURVE ( 'NONE', #22485, #4554, #8242, .T. ) ;
#10081 = EDGE_CURVE ( 'NONE', #23544, #22677, #14438, .T. ) ;
#10082 = CARTESIAN_POINT ( 'NONE',  ( 99.60675733924549036, 85.63108538499666622, 100.0000000000000142 ) ) ;
#10083 = VECTOR ( 'NONE', #21731, 1000.000000000000000 ) ;
#10084 = CARTESIAN_POINT ( 'NONE',  ( -28.05246235954390244, 188.0718642840173516, -13.00000000000000000 ) ) ;
#10085 = VERTEX_POINT ( 'NONE', #23468 ) ;
#10086 = EDGE_LOOP ( 'NONE', ( #7885, #14505, #2642, #13298 ) ) ;
#10087 = CARTESIAN_POINT ( 'NONE',  ( 158.0000000000004263, 166.3346248423521274, 45.00000000000000000 ) ) ;
#10088 = AXIS2_PLACEMENT_3D ( 'NONE', #2822, #11616, #16062 ) ;
#10089 = DIRECTION ( 'NONE',  ( 0.000000000000000000, 0.000000000000000000, 1.000000000000000000 ) ) ;
#10090 = CARTESIAN_POINT ( 'NONE',  ( 157.9999999999998295, 229.0315000300280417, 45.00000000000000000 ) ) ;
#10091 = VERTEX_POINT ( 'NONE', #3641 ) ;
#10092 = CARTESIAN_POINT ( 'NONE',  ( 118.9718481642008641, 125.5986290015192708, 100.0000000000000142 ) ) ;
#10093 = ORIENTED_EDGE ( 'NONE', *, *, #8488, .F. ) ;
#10094 = FACE_OUTER_BOUND ( 'NONE', #11068, .T. ) ;
#10095 = CARTESIAN_POINT ( 'NONE',  ( -54.22951502486254327, 83.26691194124390449, 45.00000000000000000 ) ) ;
#10096 = PLANE ( 'NONE',  #10303 ) ;
#10097 = CARTESIAN_POINT ( 'NONE',  ( 158.0000000000002274, 183.8897498949014278, 45.00000000000000000 ) ) ;
#10098 = CARTESIAN_POINT ( 'NONE',  ( 157.4999999999998579, 176.1121873686267350, -45.00000000000000000 ) ) ;
#10099 = ADVANCED_FACE ( 'NONE', ( #25755 ), #3923, .T. ) ;
#10100 = EDGE_CURVE ( 'NONE', #7159, #2485, #16729, .T. ) ;
#10101 = LINE ( 'NONE', #14844, #21142 ) ;
#10102 = CARTESIAN_POINT ( 'NONE',  ( 162.6214317851641908, 208.2882202355792742, -149.7646631383025237 ) ) ;
#10103 = EDGE_LOOP ( 'NONE', ( #23265, #17570, #25522, #10985, #9939 ) ) ;
#10104 = AXIS2_PLACEMENT_3D ( 'NONE', #3373, #7833, #27913 ) ;
#10105 = DIRECTION ( 'NONE',  ( -0.000000000000000000, -0.000000000000000000, 1.000000000000000000 ) ) ;
#10106 = EDGE_CURVE ( 'NONE', #24140, #22209, #18873, .T. ) ;
#10107 =( BOUNDED_SURFACE ( )  B_SPLINE_SURFACE ( 3, 2, ( 
 ( #13985, #13838, #16130 ),
 ( #4905, #9519, #2901 ),
 ( #1024, #24880, #5194 ),
 ( #5335, #7642, #18415 ),
 ( #11543, #11686, #22441 ),
 ( #752, #25154, #18276 ),
 ( #16407, #22729, #3033 ),
 ( #11821, #20561, #27166 ),
 ( #16269, #11959, #25022 ),
 ( #14114, #2751, #22863 ),
 ( #3169, #20702, #9798 ),
 ( #18554, #5472, #24598 ),
 ( #26544, #26843, #4568 ),
 ( #17939, #7168, #19666 ),
 ( #18089, #22391, #2704 ),
 ( #6875, #15373, #15941 ),
 ( #9180, #7019, #2270 ),
 ( #562, #24128, #24690 ),
 ( #419, #2411, #26689 ),
 ( #13497, #20087, #19804 ),
 ( #4999, #9325, #12967 ),
 ( #2557, #24546, #11490 ),
 ( #279, #22246, #21827 ),
 ( #19947, #20232, #11194 ),
 ( #4855, #15805, #2133 ),
 ( #13644, #17502, #26268 ),
 ( #10907, #128, #8752 ),
 ( #6594, #4429, #15655 ),
 ( #13214, #24401, #21959 ),
 ( #11051, #8894, #17651 ),
 ( #13355, #26405, #9038 ),
 ( #17788, #6728, #11343 ),
 ( #22105, #4712, #15512 ),
 ( #24260, #9475, #16225 ),
 ( #16638, #7311, #7456 ),
 ( #20801, #18231, #25393 ),
 ( #26978, #3408, #20377 ),
 ( #705, #16086, #25251 ),
 ( #842, #18370, #27529 ),
 ( #14072, #2987, #16364 ),
 ( #9611, #24837, #5147 ),
 ( #5570, #14210, #27123 ),
 ( #7869, #9753, #22823 ),
 ( #25108, #18647, #24976 ),
 ( #22538, #27390, #20519 ),
 ( #13937, #13791, #5289 ) ),
 .UNSPECIFIED., .F., .F., .T. ) 
 B_SPLINE_SURFACE_WITH_KNOTS ( ( 4, 2, 2, 2, 2, 2, 2, 2, 2, 2, 2, 2, 2, 2, 2, 2, 2, 2, 2, 2, 2, 2, 4 ),
 ( 3, 3 ),
 ( 1.734723475976807094E-18, 0.004062158184156357439, 0.008124316368312713144, 0.01015539546039089143, 0.01218647455246906972, 0.01624863273662542629, 0.01827971182870360284, 0.02031079092078178286, 0.02437294910493813943, 0.02640402819701631598, 0.02843510728909449600, 0.03249726547325085257, 0.03655942365740720568, 0.03859050274948538917, 0.04062158184156356572, 0.04468374002571992576, 0.04874589820987627886, 0.05280805639403263196, 0.05687021457818899201, 0.05890129367026716856, 0.06093237276234535205, 0.06296345185442353554, 0.06499453094650170515 ),
 ( 0.000000000000000000, 1.000000000000000000 ),
 .UNSPECIFIED. ) 
 GEOMETRIC_REPRESENTATION_ITEM ( )  RATIONAL_B_SPLINE_SURFACE ( (
 ( 1.000000000000000000, 0.7071067811865475727, 1.000000000000000000),
 ( 1.000000000000000000, 0.7127618277282585790, 1.000000000000000000),
 ( 1.000000000000000000, 0.7177019917272278171, 1.000000000000000000),
 ( 1.000000000000000000, 0.7259809929038707477, 1.000000000000000000),
 ( 1.000000000000000000, 0.7293222386929405499, 1.000000000000000000),
 ( 1.000000000000000000, 0.7329411530155929277, 1.000000000000000000),
 ( 1.000000000000000000, 0.7339161091547746762, 1.000000000000000000),
 ( 1.000000000000000000, 0.7353380047207397352, 1.000000000000000000),
 ( 1.000000000000000000, 0.7357895841719410690, 1.000000000000000000),
 ( 1.000000000000000000, 0.7363489957920964502, 1.000000000000000000),
 ( 1.000000000000000000, 0.7356640979630035826, 1.000000000000000000),
 ( 1.000000000000000000, 0.7329334158298154156, 1.000000000000000000),
 ( 1.000000000000000000, 0.7317386460502656176, 1.000000000000000000),
 ( 1.000000000000000000, 0.7287527534627166181, 1.000000000000000000),
 ( 1.000000000000000000, 0.7269678409236182137, 1.000000000000000000),
 ( 1.000000000000000000, 0.7207930214942670499, 1.000000000000000000),
 ( 1.000000000000000000, 0.7155672824331827941, 1.000000000000000000),
 ( 1.000000000000000000, 0.7060917826293187094, 1.000000000000000000),
 ( 1.000000000000000000, 0.7026601427810345024, 1.000000000000000000),
 ( 1.000000000000000000, 0.6952527892509122731, 1.000000000000000000),
 ( 1.000000000000000000, 0.6912624871066671561, 1.000000000000000000),
 ( 1.000000000000000000, 0.6786163957654665069, 1.000000000000000000),
 ( 1.000000000000000000, 0.6692836425642715303, 1.000000000000000000),
 ( 1.000000000000000000, 0.6490371914780060925, 1.000000000000000000),
 ( 1.000000000000000000, 0.6381215166341221989, 1.000000000000000000),
 ( 1.000000000000000000, 0.6207537710089482408, 1.000000000000000000),
 ( 1.000000000000000000, 0.6147992736454299667, 1.000000000000000000),
 ( 1.000000000000000000, 0.6026007117946927671, 1.000000000000000000),
 ( 1.000000000000000000, 0.5963421480515447293, 1.000000000000000000),
 ( 1.000000000000000000, 0.5773189341491167248, 1.000000000000000000),
 ( 1.000000000000000000, 0.5643376819677715650, 1.000000000000000000),
 ( 1.000000000000000000, 0.5383412250591570469, 1.000000000000000000),
 ( 1.000000000000000000, 0.5253226519624610846, 1.000000000000000000),
 ( 1.000000000000000000, 0.5000277150692035155, 1.000000000000000000),
 ( 1.000000000000000000, 0.4877436159665405335, 1.000000000000000000),
 ( 1.000000000000000000, 0.4650351994093656072, 1.000000000000000000),
 ( 1.000000000000000000, 0.4547962088601842923, 1.000000000000000000),
 ( 1.000000000000000000, 0.4420154047700521338, 1.000000000000000000),
 ( 1.000000000000000000, 0.4381857281609657373, 1.000000000000000000),
 ( 1.000000000000000000, 0.4315381087321277787, 1.000000000000000000),
 ( 1.000000000000000000, 0.4287205967313478805, 1.000000000000000000),
 ( 1.000000000000000000, 0.4242344318730199015, 1.000000000000000000),
 ( 1.000000000000000000, 0.4225662398543922893, 1.000000000000000000),
 ( 1.000000000000000000, 0.4204880647989017173, 1.000000000000000000),
 ( 1.000000000000000000, 0.4200800889062838439, 1.000000000000000000),
 ( 1.000000000000000000, 0.4203293914240995299, 1.000000000000000000) ) ) 
 REPRESENTATION_ITEM ( '' )  SURFACE ( )  );
#10108 = LINE ( 'NONE', #15921, #3227 ) ;
#10109 = DIRECTION ( 'NONE',  ( 0.4528218681380702382, -0.8916010070294605461, 0.000000000000000000 ) ) ;
#10110 = CARTESIAN_POINT ( 'NONE',  ( -56.48697296830715686, 1.968917815184006985E-15, 99.00000000000000000 ) ) ;
#10111 = ORIENTED_EDGE ( 'NONE', *, *, #15112, .F. ) ;
#10112 = LINE ( 'NONE', #10252, #14194 ) ;
#10113 = AXIS2_PLACEMENT_3D ( 'NONE', #7955, #20603, #5658 ) ;
#10114 = ORIENTED_EDGE ( 'NONE', *, *, #7316, .T. ) ;
#10115 = AXIS2_PLACEMENT_3D ( 'NONE', #25000, #7341, #11804 ) ;
#10116 = FACE_OUTER_BOUND ( 'NONE', #11901, .T. ) ;
#10117 = DIRECTION ( 'NONE',  ( 1.000000000000000000, -0.000000000000000000, -0.000000000000000000 ) ) ;
#10118 = CARTESIAN_POINT ( 'NONE',  ( 135.7863972241894430, 249.9903379835593853, -139.0484678162419812 ) ) ;
#10119 = EDGE_LOOP ( 'NONE', ( #6081, #15248 ) ) ;
#10120 = CARTESIAN_POINT ( 'NONE',  ( 157.4999999999998010, 241.3169375638095460, 45.00000000000000000 ) ) ;
#10121 = CARTESIAN_POINT ( 'NONE',  ( 134.9999999999998579, 220.0000000000000284, -90.00000000000002842 ) ) ;
#10122 = ORIENTED_EDGE ( 'NONE', *, *, #15075, .T. ) ;
#10123 = DIRECTION ( 'NONE',  ( -0.000000000000000000, -0.000000000000000000, -1.000000000000000000 ) ) ;
#10124 = CARTESIAN_POINT ( 'NONE',  ( 108.6430962847606736, 252.6780396303561247, 32.26456250497143685 ) ) ;
#10125 = ORIENTED_EDGE ( 'NONE', *, *, #19407, .T. ) ;
#10126 = VERTEX_POINT ( 'NONE', #12429 ) ;
#10127 = CARTESIAN_POINT ( 'NONE',  ( 232.4999999999996305, 186.4134324495536248, 35.02193266779035952 ) ) ;
#10128 = EDGE_LOOP ( 'NONE', ( #20785, #13926, #404, #24430 ) ) ;
#10129 = VECTOR ( 'NONE', #11708, 1000.000000000000000 ) ;
#10130 = ORIENTED_EDGE ( 'NONE', *, *, #21243, .T. ) ;
#10131 = ORIENTED_EDGE ( 'NONE', *, *, #4797, .T. ) ;
#10132 = CARTESIAN_POINT ( 'NONE',  ( 2.399999999999999911, 0.000000000000000000, -7.685040811306673270 ) ) ;
#10133 = AXIS2_PLACEMENT_3D ( 'NONE', #6572, #18859, #14283 ) ;
#10134 = LINE ( 'NONE', #25213, #9430 ) ;
#10135 = EDGE_CURVE ( 'NONE', #18450, #12823, #21168, .T. ) ;
#10136 = CARTESIAN_POINT ( 'NONE',  ( 158.0000000000004547, 165.8267498348450886, 45.00000000000000000 ) ) ;
#10137 = EDGE_CURVE ( 'NONE', #18830, #10085, #15709, .T. ) ;
#10138 = CARTESIAN_POINT ( 'NONE',  ( 157.4999999999998579, 196.1751874286831026, -45.00000000000000000 ) ) ;
#10139 = CARTESIAN_POINT ( 'NONE',  ( 127.3463313526982716, 201.5224093497739943, -45.00000000000000000 ) ) ;
#10140 = DIRECTION ( 'NONE',  ( -0.8916010070299780210, -0.4528218681370510534, 0.000000000000000000 ) ) ;
#10141 = EDGE_CURVE ( 'NONE', #2873, #18634, #4343, .T. ) ;
#10142 = LINE ( 'NONE', #13428, #16369 ) ;
#10143 = CARTESIAN_POINT ( 'NONE',  ( 158.0000000000005684, 153.2873747973098659, -45.00000000000000000 ) ) ;
#10144 = DIRECTION ( 'NONE',  ( 0.8916010070299267287, -0.4528218681371523058, 0.000000000000000000 ) ) ;
#10145 = CARTESIAN_POINT ( 'NONE',  ( -217.0264852877946566, -91.18033988749901653, 0.000000000000000000 ) ) ;
#10146 = ORIENTED_EDGE ( 'NONE', *, *, #13882, .F. ) ;
#10147 = LINE ( 'NONE', #17170, #13730 ) ;
#10148 = AXIS2_PLACEMENT_3D ( 'NONE', #23309, #5921, #25735 ) ;
#10149 = CARTESIAN_POINT ( 'NONE',  ( 157.4999999999996589, 276.4271876689075498, 45.00000000000000000 ) ) ;
#10150 = CARTESIAN_POINT ( 'NONE',  ( 26.84558326594468625, 84.84596205450714024, 99.61258732158417217 ) ) ;
#10151 = DIRECTION ( 'NONE',  ( -1.000000000000000000, 0.000000000000000000, 0.000000000000000000 ) ) ;
#10152 = CARTESIAN_POINT ( 'NONE',  ( 158.0000000000005684, 151.2873747973098659, -45.00000000000000000 ) ) ;
#10153 = ORIENTED_EDGE ( 'NONE', *, *, #7890, .T. ) ;
#10154 = VECTOR ( 'NONE', #18822, 1000.000000000000000 ) ;
#10155 = DIRECTION ( 'NONE',  ( 0.000000000000000000, 1.000000000000000000, 0.000000000000000000 ) ) ;
#10156 = VERTEX_POINT ( 'NONE', #2612 ) ;
#10157 = LINE ( 'NONE', #1388, #22734 ) ;
#10158 = ORIENTED_EDGE ( 'NONE', *, *, #2169, .F. ) ;
#10159 = ORIENTED_EDGE ( 'NONE', *, *, #6593, .T. ) ;
#10160 = CARTESIAN_POINT ( 'NONE',  ( -52.82053747318527570, 131.8412021680207431, 16.12000459196658397 ) ) ;
#10161 = ORIENTED_EDGE ( 'NONE', *, *, #3175, .F. ) ;
#10162 = ORIENTED_EDGE ( 'NONE', *, *, #26141, .T. ) ;
#10163 = DIRECTION ( 'NONE',  ( -0.000000000000000000, -0.000000000000000000, -1.000000000000000000 ) ) ;
#10164 = CARTESIAN_POINT ( 'NONE',  ( -189.8086322075389774, 92.49158130768422836, 12.99999999999999822 ) ) ;
#10165 = CARTESIAN_POINT ( 'NONE',  ( 157.4999999999998579, 65.76568703831686946, 45.00000000000000000 ) ) ;
#10166 = ADVANCED_FACE ( 'NONE', ( #9235 ), #26321, .F. ) ;
#10167 = VECTOR ( 'NONE', #19774, 1000.000000000000000 ) ;
#10168 = CARTESIAN_POINT ( 'NONE',  ( -134.9821047572740156, 129.7556574183901432, -16.76521942151183708 ) ) ;
#10169 = VECTOR ( 'NONE', #23188, 1000.000000000000000 ) ;
#10170 = EDGE_CURVE ( 'NONE', #17928, #27752, #26180, .T. ) ;
#10171 = FACE_OUTER_BOUND ( 'NONE', #14440, .T. ) ;
#10172 = DIRECTION ( 'NONE',  ( 0.8916010070294699830, -0.4528218681380514199, 0.000000000000000000 ) ) ;
#10173 = CARTESIAN_POINT ( 'NONE',  ( -270.0681032424402588, -170.3775688406267363, 93.68413306229582815 ) ) ;
#10174 = EDGE_CURVE ( 'NONE', #3224, #301, #17563, .T. ) ;
#10175 = LINE ( 'NONE', #21224, #20929 ) ;
#10176 = CARTESIAN_POINT ( 'NONE',  ( -205.4481996895170539, 90.78692297191672367, 28.57879081633423368 ) ) ;
#10177 = CARTESIAN_POINT ( 'NONE',  ( 157.4999999999998579, 60.74993702330277756, -45.00000000000000000 ) ) ;
#10178 = PLANE ( 'NONE',  #9081 ) ;
#10179 = DIRECTION ( 'NONE',  ( 0.000000000000000000, 0.000000000000000000, -1.000000000000000000 ) ) ;
#10180 = EDGE_LOOP ( 'NONE', ( #28008, #18255, #4174, #16522 ) ) ;
#10181 = CARTESIAN_POINT ( 'NONE',  ( -210.0000000000000568, -152.0000000000000284, -110.0000000000000284 ) ) ;
#10182 = LINE ( 'NONE', #1830, #25294 ) ;
#10184 = ORIENTED_EDGE ( 'NONE', *, *, #10666, .F. ) ;
#10183 = VERTEX_POINT ( 'NONE', #8666 ) ;
#10185 = VECTOR ( 'NONE', #15167, 1000.000000000000114 ) ;
#10186 = CARTESIAN_POINT ( 'NONE',  ( -12.00299901279919723, 223.4254219457707222, -45.00000000000000000 ) ) ;
#10187 = ORIENTED_EDGE ( 'NONE', *, *, #16555, .T. ) ;
#10188 = ORIENTED_EDGE ( 'NONE', *, *, #17648, .T. ) ;
#10189 = CIRCLE ( 'NONE', #26231, 9.999999999999991118 ) ;
#10190 =( GEOMETRIC_REPRESENTATION_CONTEXT ( 3 ) GLOBAL_UNCERTAINTY_ASSIGNED_CONTEXT ( ( #4295 ) ) GLOBAL_UNIT_ASSIGNED_CONTEXT ( ( #4198, #19579, #15424 ) ) REPRESENTATION_CONTEXT ( 'NONE', 'WORKASPACE' ) );
#10191 = ORIENTED_EDGE ( 'NONE', *, *, #5812, .T. ) ;
#10192 = TOROIDAL_SURFACE ( 'NONE', #16174, 11.00000000000001066, 1.000000000000000000 ) ;
#10193 = ORIENTED_EDGE ( 'NONE', *, *, #12476, .T. ) ;
#10194 = EDGE_CURVE ( 'NONE', #22091, #8949, #17978, .T. ) ;
#10195 = ORIENTED_EDGE ( 'NONE', *, *, #21022, .T. ) ;
#10196 = VERTEX_POINT ( 'NONE', #20001 ) ;
#10197 = PLANE ( 'NONE',  #27845 ) ;
#10198 = EDGE_CURVE ( 'NONE', #2939, #19703, #17422, .T. ) ;
#10199 = DIRECTION ( 'NONE',  ( 0.000000000000000000, -1.000000000000000000, 0.000000000000000000 ) ) ;
#10200 = LINE ( 'NONE', #1708, #7043 ) ;
#10201 = AXIS2_PLACEMENT_3D ( 'NONE', #14127, #23435, #1316 ) ;
#10202 = CARTESIAN_POINT ( 'NONE',  ( -7.973710589631370027, 131.1492272393548433, -16.33314721351600340 ) ) ;
#10203 = TOROIDAL_SURFACE ( 'NONE', #16629, 11.00000000000001066, 1.000000000000000000 ) ;
#10204 = EDGE_CURVE ( 'NONE', #24279, #14031, #12993, .T. ) ;
#10205 = DIRECTION ( 'NONE',  ( -0.000000000000000000, -0.000000000000000000, 1.000000000000000000 ) ) ;
#10206 = FACE_OUTER_BOUND ( 'NONE', #16452, .T. ) ;
#10207 = CARTESIAN_POINT ( 'NONE',  ( -248.1546605714623013, -91.18033988749901653, 10.70611877156249214 ) ) ;
#10208 = VECTOR ( 'NONE', #9910, 1000.000000000000000 ) ;
#10209 = EDGE_CURVE ( 'NONE', #13594, #26578, #9088, .T. ) ;
#10210 = DIRECTION ( 'NONE',  ( 0.000000000000000000, 0.000000000000000000, -1.000000000000000000 ) ) ;
#10211 = DIRECTION ( 'NONE',  ( -0.000000000000000000, -9.208809080520486542E-17, 1.000000000000000000 ) ) ;
#10212 = FACE_OUTER_BOUND ( 'NONE', #25862, .T. ) ;
#10213 = CARTESIAN_POINT ( 'NONE',  ( 157.9999999999997158, 256.6181251126050711, -45.00000000000000000 ) ) ;
#10214 = ORIENTED_EDGE ( 'NONE', *, *, #12857, .F. ) ;
#10215 = DIRECTION ( 'NONE',  ( -0.8916010070293483025, -0.4528218681382912281, 0.000000000000000000 ) ) ;
#10216 = VERTEX_POINT ( 'NONE', #6504 ) ;
#10217 = PRODUCT_CONTEXT ( 'NONE', #5603, 'mechanical' ) ;
#10218 = ORIENTED_EDGE ( 'NONE', *, *, #21742, .T. ) ;
#10219 = EDGE_CURVE ( 'NONE', #18978, #19273, #21739, .T. ) ;
#10220 = AXIS2_PLACEMENT_3D ( 'NONE', #14972, #19268, #10089 ) ;
#10221 = ORIENTED_EDGE ( 'NONE', *, *, #7225, .T. ) ;
#10222 = VECTOR ( 'NONE', #21907, 1000.000000000000000 ) ;
#10223 = CARTESIAN_POINT ( 'NONE',  ( 118.9718481642008641, 125.5986290015192708, 100.0000000000000142 ) ) ;
#10224 = LINE ( 'NONE', #3319, #26892 ) ;
#10225 = ORIENTED_EDGE ( 'NONE', *, *, #25881, .T. ) ;
#10226 = AXIS2_PLACEMENT_3D ( 'NONE', #26277, #1999, #17509 ) ;
#10227 = ORIENTED_EDGE ( 'NONE', *, *, #19364, .T. ) ;
#10228 = CARTESIAN_POINT ( 'NONE',  ( 157.9999999999996305, 284.2047501951820436, -45.00000000000000000 ) ) ;
#10229 = VECTOR ( 'NONE', #11036, 1000.000000000000114 ) ;
#10230 = EDGE_CURVE ( 'NONE', #27270, #28324, #14316, .T. ) ;
#10231 = CARTESIAN_POINT ( 'NONE',  ( 432.4999999999996589, -5.589247009368160768, 100.0000000000000426 ) ) ;
#10232 = DIRECTION ( 'NONE',  ( 2.220446049250266932E-15, -0.000000000000000000, 1.000000000000000000 ) ) ;
#10233 = EDGE_LOOP ( 'NONE', ( #13581, #13118, #6582, #24032 ) ) ;
#10234 = DIRECTION ( 'NONE',  ( 0.3825563754725206378, 0.000000000000000000, -0.9239321509641971186 ) ) ;
#10235 = ORIENTED_EDGE ( 'NONE', *, *, #5464, .F. ) ;
#10236 = CARTESIAN_POINT ( 'NONE',  ( 132.3894761555988282, 239.8288972274758919, 45.00000000000000000 ) ) ;
#10237 = LINE ( 'NONE', #16842, #23670 ) ;
#10238 = CARTESIAN_POINT ( 'NONE',  ( -524.0002167759885197, -169.4627935898112696, 0.000000000000000000 ) ) ;
#10239 = LINE ( 'NONE', #23169, #6239 ) ;
#10240 = DIRECTION ( 'NONE',  ( 4.625929269271489858E-16, 0.000000000000000000, 1.000000000000000000 ) ) ;
#10241 = VECTOR ( 'NONE', #5913, 1000.000000000000114 ) ;
#10242 = EDGE_CURVE ( 'NONE', #6712, #22236, #42, .T. ) ;
#10243 = PLANE ( 'NONE',  #27999 ) ;
#10244 = DIRECTION ( 'NONE',  ( -0.8916010070293409751, -0.4528218681383056610, 0.000000000000000000 ) ) ;
#10245 = ORIENTED_EDGE ( 'NONE', *, *, #6781, .F. ) ;
#10246 = EDGE_CURVE ( 'NONE', #12285, #18364, #4620, .T. ) ;
#10247 = CARTESIAN_POINT ( 'NONE',  ( -41.04971513216914047, 194.3765543069588659, -45.00000000000000000 ) ) ;
#10248 = DIRECTION ( 'NONE',  ( 1.000000000000000000, -0.000000000000000000, -0.000000000000000000 ) ) ;
#10249 = AXIS2_PLACEMENT_3D ( 'NONE', #13192, #103, #26097 ) ;
#10250 = CARTESIAN_POINT ( 'NONE',  ( 158.0000000000015632, 55.98812451204224061, -45.00000000000000000 ) ) ;
#10251 = ORIENTED_EDGE ( 'NONE', *, *, #24504, .T. ) ;
#10252 = CARTESIAN_POINT ( 'NONE',  ( -112.3221550338875687, 17.24192588826928585, 83.00000000000001421 ) ) ;
#10253 = ORIENTED_EDGE ( 'NONE', *, *, #27367, .T. ) ;
#10254 = CARTESIAN_POINT ( 'NONE',  ( -201.6077923708984656, 94.40672121051507304, 29.51043390529410004 ) ) ;
#10255 = DIRECTION ( 'NONE',  ( -1.000000000000000000, 0.000000000000000000, 3.053113317719176147E-15 ) ) ;
#10256 = CARTESIAN_POINT ( 'NONE',  ( -230.8252095005209128, 92.50430350379889433, 12.99999999999994849 ) ) ;
#10257 = ORIENTED_EDGE ( 'NONE', *, *, #22618, .T. ) ;
#10258 = DIRECTION ( 'NONE',  ( -1.000000000000000000, 0.000000000000000000, 0.000000000000000000 ) ) ;
#10259 = ORIENTED_EDGE ( 'NONE', *, *, #24097, .F. ) ;
#10260 = ADVANCED_FACE ( 'NONE', ( #24040 ), #4202, .F. ) ;
#10261 = CARTESIAN_POINT ( 'NONE',  ( -160.0000000000000284, 119.7660240611718763, 22.85081902853005431 ) ) ;
#10262 = CARTESIAN_POINT ( 'NONE',  ( 107.1322492465393736, 249.6642686020492476, 26.92713756708314321 ) ) ;
#10263 = ORIENTED_EDGE ( 'NONE', *, *, #3005, .F. ) ;
#10264 = AXIS2_PLACEMENT_3D ( 'NONE', #22425, #15977, #13970 ) ;
#10265 = ORIENTED_EDGE ( 'NONE', *, *, #11291, .T. ) ;
#10266 = EDGE_CURVE ( 'NONE', #9316, #9424, #22160, .T. ) ;
#10267 = FACE_OUTER_BOUND ( 'NONE', #1738, .T. ) ;
#10268 = ORIENTED_EDGE ( 'NONE', *, *, #3737, .F. ) ;
#10269 = VECTOR ( 'NONE', #8940, 1000.000000000000227 ) ;
#10270 = EDGE_CURVE ( 'NONE', #372, #1220, #8801, .T. ) ;
#10271 = ORIENTED_EDGE ( 'NONE', *, *, #1640, .T. ) ;
#10272 = ORIENTED_EDGE ( 'NONE', *, *, #17716, .F. ) ;
#10273 = AXIS2_PLACEMENT_3D ( 'NONE', #13580, #22330, #26923 ) ;
#10274 = FACE_OUTER_BOUND ( 'NONE', #15409, .T. ) ;
#10275 = CARTESIAN_POINT ( 'NONE',  ( -227.8378063125350650, 130.6400894613935293, 12.99999999999999822 ) ) ;
#10276 = DIRECTION ( 'NONE',  ( 0.000000000000000000, -1.387778780781445429E-16, -1.000000000000000000 ) ) ;
#10277 = SHAPE_REPRESENTATION ( 'Gear Rack', ( #10637 ), #15244 ) ;
#10278 = CARTESIAN_POINT ( 'NONE',  ( 115.6411010564591777, 208.5333949359988139, -99.00000000000001421 ) ) ;
#10279 = FACE_OUTER_BOUND ( 'NONE', #8910, .T. ) ;
#10280 = FACE_OUTER_BOUND ( 'NONE', #14936, .T. ) ;
#10281 = CARTESIAN_POINT ( 'NONE',  ( 1.633516369018861658, 1.249999999999999556, -7.514731128045610831 ) ) ;
#10282 = CARTESIAN_POINT ( 'NONE',  ( 158.0000000000002842, 180.8739998798873501, -45.00000000000000000 ) ) ;
#10283 = LINE ( 'NONE', #14458, #8176 ) ;
#10284 = DIRECTION ( 'NONE',  ( -0.8916010070297953893, -0.4528218681374107657, 0.000000000000000000 ) ) ;
#10285 = VERTEX_POINT ( 'NONE', #15563 ) ;
#10286 = AXIS2_PLACEMENT_3D ( 'NONE', #13568, #6939, #17575 ) ;
#10287 = LINE ( 'NONE', #19178, #10044 ) ;
#10288 = CARTESIAN_POINT ( 'NONE',  ( 97.02586881228830862, 241.2701687844766809, -10.66912238342227681 ) ) ;
#10289 = CARTESIAN_POINT ( 'NONE',  ( 20.33006372853257560, 88.24318430726339102, 98.85875548193735085 ) ) ;
#10290 = DIRECTION ( 'NONE',  ( -0.000000000000000000, -0.000000000000000000, -1.000000000000000000 ) ) ;
#10291 = VECTOR ( 'NONE', #14562, 1000.000000000000114 ) ;
#10292 = ORIENTED_EDGE ( 'NONE', *, *, #25428, .T. ) ;
#10293 = ORIENTED_EDGE ( 'NONE', *, *, #20668, .T. ) ;
#10294 = CARTESIAN_POINT ( 'NONE',  ( 65.00000000000000000, -150.0000000000000568, 70.00000000000001421 ) ) ;
#10295 = ORIENTED_EDGE ( 'NONE', *, *, #20447, .F. ) ;
#10296 = EDGE_CURVE ( 'NONE', #13033, #22331, #16610, .T. ) ;
#10297 = EDGE_LOOP ( 'NONE', ( #27315, #2145, #26572, #25206 ) ) ;
#10298 = EDGE_CURVE ( 'NONE', #27610, #25616, #2466, .T. ) ;
#10299 = CARTESIAN_POINT ( 'NONE',  ( -82.72216334395888282, 136.4210859576436974, 13.48999651779888254 ) ) ;
#10300 = EDGE_LOOP ( 'NONE', ( #12225, #22302 ) ) ;
#10301 = ORIENTED_EDGE ( 'NONE', *, *, #8113, .F. ) ;
#10302 = CARTESIAN_POINT ( 'NONE',  ( 114.6860526936801534, 210.2756460775362086, 98.48425370696797643 ) ) ;
#10303 = AXIS2_PLACEMENT_3D ( 'NONE', #18851, #24764, #5071 ) ;
#10304 = CARTESIAN_POINT ( 'NONE',  ( -150.9620302853898295, 123.3689204320809125, -20.02690237861579803 ) ) ;
#10305 = CARTESIAN_POINT ( 'NONE',  ( 157.4999999999998295, 231.2854375337815327, -45.00000000000000000 ) ) ;
#10306 = PLANE ( 'NONE',  #11935 ) ;
#10307 = VECTOR ( 'NONE', #12457, 999.9999999999998863 ) ;
#10308 = CARTESIAN_POINT ( 'NONE',  ( -266.3442505907551663, -165.6659793133063374, -89.32861420273920317 ) ) ;
#10309 = CARTESIAN_POINT ( 'NONE',  ( -225.7036482868739427, -91.18033988749901653, 0.000000000000000000 ) ) ;
#10310 = CARTESIAN_POINT ( 'NONE',  ( 19.81673173095627050, -48.35333013564442695, 98.81407962859346128 ) ) ;
#10311 = CARTESIAN_POINT ( 'NONE',  ( -220.2847051492696551, 86.26875468262431923, -18.58588010854248651 ) ) ;
#10312 = EDGE_CURVE ( 'NONE', #16161, #19401, #3318, .T. ) ;
#10313 = CARTESIAN_POINT ( 'NONE',  ( 129.1547762805313937, 249.4250724608095595, -143.6319245046325079 ) ) ;
#10314 = CARTESIAN_POINT ( 'NONE',  ( -208.8144187295359302, 88.72373865873345267, 26.17480155654782337 ) ) ;
#10315 = PLANE ( 'NONE',  #8782 ) ;
#10316 = CARTESIAN_POINT ( 'NONE',  ( -160.0000000000000284, 79.99999999999994316, -70.00000000000001421 ) ) ;
#10317 = DIRECTION ( 'NONE',  ( 1.000000000000000000, 0.000000000000000000, 0.000000000000000000 ) ) ;
#10318 = ORIENTED_EDGE ( 'NONE', *, *, #24047, .F. ) ;
#10319 = EDGE_CURVE ( 'NONE', #16689, #15640, #2377, .T. ) ;
#10320 = LINE ( 'NONE', #5581, #4091 ) ;
#10321 = DIRECTION ( 'NONE',  ( 0.000000000000000000, 0.000000000000000000, -1.000000000000000000 ) ) ;
#10323 = ORIENTED_EDGE ( 'NONE', *, *, #1773, .T. ) ;
#10322 = ORIENTED_EDGE ( 'NONE', *, *, #10651, .T. ) ;
#10324 = VECTOR ( 'NONE', #19532, 1000.000000000000000 ) ;
#10325 = CARTESIAN_POINT ( 'NONE',  ( 106.0806716805053611, 248.0923932631361595, -24.09863730005714544 ) ) ;
#10326 = ORIENTED_EDGE ( 'NONE', *, *, #17650, .F. ) ;
#10327 = ORIENTED_EDGE ( 'NONE', *, *, #3892, .F. ) ;
#10328 = EDGE_CURVE ( 'NONE', #19372, #8066, #18459, .T. ) ;
#10329 = VECTOR ( 'NONE', #7816, 1000.000000000000227 ) ;
#10330 = VERTEX_POINT ( 'NONE', #2756 ) ;
#10331 = EDGE_CURVE ( 'NONE', #13726, #8797, #759, .T. ) ;
#10332 = EDGE_CURVE ( 'NONE', #12221, #3706, #10189, .T. ) ;
#10333 = ORIENTED_EDGE ( 'NONE', *, *, #27848, .T. ) ;
#10334 = ORIENTED_EDGE ( 'NONE', *, *, #10353, .T. ) ;
#10335 = ORIENTED_EDGE ( 'NONE', *, *, #26233, .T. ) ;
#10336 = DIRECTION ( 'NONE',  ( 0.000000000000000000, -1.000000000000000000, -1.214306433183764966E-16 ) ) ;
#10337 = LINE ( 'NONE', #23552, #17859 ) ;
#10338 = AXIS2_PLACEMENT_3D ( 'NONE', #3675, #5836, #14330 ) ;
#10339 = CARTESIAN_POINT ( 'NONE',  ( 157.9999999999997158, 259.1260001201120531, 45.00000000000000000 ) ) ;
#10340 = CARTESIAN_POINT ( 'NONE',  ( -0.4949115998893022783, 134.1005191953554743, -15.57096562799038963 ) ) ;
#10341 = CARTESIAN_POINT ( 'NONE',  ( 232.4999999999996305, 194.4107529906318064, -62.90796922943941638 ) ) ;
#10342 = VECTOR ( 'NONE', #4359, 1000.000000000000000 ) ;
#10343 = CARTESIAN_POINT ( 'NONE',  ( 158.0000000000014211, 68.52749954957745615, 45.00000000000000000 ) ) ;
#10344 = CARTESIAN_POINT ( 'NONE',  ( -207.5044420441007560, 75.59897387903043864, -44.47015349860520672 ) ) ;
#10345 = CARTESIAN_POINT ( 'NONE',  ( 157.4999999999998579, 156.0491873085704242, 45.00000000000000000 ) ) ;
#10346 = CARTESIAN_POINT ( 'NONE',  ( 158.0000000000011084, 100.6219996396619791, -45.00000000000000000 ) ) ;
#10347 = DIRECTION ( 'NONE',  ( 0.000000000000000000, -1.000000000000000000, 0.000000000000000000 ) ) ;
#10348 = CARTESIAN_POINT ( 'NONE',  ( 158.0000000000014779, 63.51174953456337136, 45.00000000000000000 ) ) ;
#10349 = ORIENTED_EDGE ( 'NONE', *, *, #18672, .F. ) ;
#10350 = CARTESIAN_POINT ( 'NONE',  ( 372.9108539694884144, 19.41075299063184900, 87.99671038392668265 ) ) ;
#10351 = EDGE_CURVE ( 'NONE', #23194, #1111, #25030, .T. ) ;
#10352 = EDGE_CURVE ( 'NONE', #4162, #23149, #22735, .T. ) ;
#10353 = EDGE_CURVE ( 'NONE', #15277, #23733, #12110, .T. ) ;
#10354 = PLANE ( 'NONE',  #22739 ) ;
#10355 = VERTEX_POINT ( 'NONE', #1171 ) ;
#10356 = AXIS2_PLACEMENT_3D ( 'NONE', #15515, #26546, #4857 ) ;
#10357 = ORIENTED_EDGE ( 'NONE', *, *, #8145, .F. ) ;
#10358 = AXIS2_PLACEMENT_3D ( 'NONE', #27360, #12445, #5958 ) ;
#10359 = VECTOR ( 'NONE', #797, 1000.000000000000000 ) ;
#10360 = VERTEX_POINT ( 'NONE', #9941 ) ;
#10361 = DIRECTION ( 'NONE',  ( -0.000000000000000000, -0.000000000000000000, -1.000000000000000000 ) ) ;
#10362 = DIRECTION ( 'NONE',  ( -1.000000000000000000, -0.000000000000000000, -0.000000000000000000 ) ) ;
#10363 = B_SPLINE_CURVE_WITH_KNOTS ( 'NONE', 3,
 ( #19926, #15208, #17483, #8872, #26247, #14922, #28108, #12912, #23962, #23818 ),
 .UNSPECIFIED., .F., .F.,
 ( 4, 2, 2, 2, 4 ),
 ( 0.000000000000000000, 0.2500000000000000000, 0.5000000000000000000, 0.7500000000000000000, 1.000000000000000000 ),
 .UNSPECIFIED. ) ;
#10364 = EDGE_CURVE ( 'NONE', #9494, #9427, #26900, .T. ) ;
#10365 = ORIENTED_EDGE ( 'NONE', *, *, #24597, .T. ) ;
#10366 = VECTOR ( 'NONE', #4573, 1000.000000000000000 ) ;
#10367 = EDGE_LOOP ( 'NONE', ( #1273, #1840, #27064, #8850 ) ) ;
#10368 = PLANE ( 'NONE',  #21879 ) ;
#10369 = DIRECTION ( 'NONE',  ( 1.000000000000000000, -0.000000000000000000, -0.000000000000000000 ) ) ;
#10370 = CARTESIAN_POINT ( 'NONE',  ( -185.9688816675270289, 106.1730371456491753, -31.51842731530989639 ) ) ;
#10371 = ORIENTED_EDGE ( 'NONE', *, *, #6731, .T. ) ;
#10372 = DIRECTION ( 'NONE',  ( 0.000000000000000000, -1.000000000000000000, 0.000000000000000000 ) ) ;
#10373 = ORIENTED_EDGE ( 'NONE', *, *, #27223, .F. ) ;
#10374 = CARTESIAN_POINT ( 'NONE',  ( 157.4999999999997442, 256.3641876088515232, -45.00000000000000000 ) ) ;
#10375 = CARTESIAN_POINT ( 'NONE',  ( -40.00387671809203738, 149.2965004116384762, 45.00000000000000000 ) ) ;
#10376 = LINE ( 'NONE', #8615, #5321 ) ;
#10377 = FACE_OUTER_BOUND ( 'NONE', #7963, .T. ) ;
#10378 = AXIS2_PLACEMENT_3D ( 'NONE', #11009, #19759, #13036 ) ;
#10379 = DIRECTION ( 'NONE',  ( 0.7059982162894324897, -0.7082136108520787898, 0.000000000000000000 ) ) ;
#10380 = CARTESIAN_POINT ( 'NONE',  ( 162.3566490199804946, 207.6824095899247880, -150.2048413890044003 ) ) ;
#10381 = EDGE_LOOP ( 'NONE', ( #11892, #13889, #9169, #16869 ) ) ;
#10382 = CARTESIAN_POINT ( 'NONE',  ( 134.9999999999998579, 220.0000000000000284, 99.00000000000001421 ) ) ;
#10384 = DIRECTION ( 'NONE',  ( -1.000000000000000000, 0.000000000000000000, -0.000000000000000000 ) ) ;
#10383 = AXIS2_PLACEMENT_3D ( 'NONE', #13290, #10844, #19602 ) ;
#10385 = DIRECTION ( 'NONE',  ( -0.8916010070297036849, 0.4528218681375913435, 0.000000000000000000 ) ) ;
#10386 = FACE_OUTER_BOUND ( 'NONE', #1616, .T. ) ;
#10387 = ORIENTED_EDGE ( 'NONE', *, *, #18850, .T. ) ;
#10388 = CARTESIAN_POINT ( 'NONE',  ( 118.3276951936840220, 235.1525654889200894, 99.88760442621966718 ) ) ;
#10389 = ADVANCED_FACE ( 'NONE', ( #7078 ), #17994, .F. ) ;
#10390 = EDGE_CURVE ( 'NONE', #27901, #14163, #18835, .T. ) ;
#10391 = APPLICATION_CONTEXT ( 'automotive_design' ) ;
#10392 = DIRECTION ( 'NONE',  ( 1.000000000000000000, 0.000000000000000000, 0.000000000000000000 ) ) ;
#10393 = LINE ( 'NONE', #12704, #26154 ) ;
#10394 = CARTESIAN_POINT ( 'NONE',  ( 350.4502000556478265, 95.60976900091161212, -145.0000000000000000 ) ) ;
#10395 = ORIENTED_EDGE ( 'NONE', *, *, #20436, .T. ) ;
#10396 = DIRECTION ( 'NONE',  ( 1.000000000000000000, 0.000000000000000000, -0.000000000000000000 ) ) ;
#10397 = CARTESIAN_POINT ( 'NONE',  ( 157.9999999999998579, 219.0000000000000284, -45.00000000000000000 ) ) ;
#10398 = VERTEX_POINT ( 'NONE', #21130 ) ;
#10399 = DIRECTION ( 'NONE',  ( 0.000000000000000000, -1.000000000000000000, 0.000000000000000000 ) ) ;
#10400 = FACE_OUTER_BOUND ( 'NONE', #784, .T. ) ;
#10401 = ORIENTED_EDGE ( 'NONE', *, *, #2599, .F. ) ;
#10402 = VECTOR ( 'NONE', #13600, 1000.000000000000000 ) ;
#10403 = ORIENTED_EDGE ( 'NONE', *, *, #13584, .T. ) ;
#10404 = PLANE ( 'NONE',  #4893 ) ;
#10405 = VERTEX_POINT ( 'NONE', #8349 ) ;
#10406 = EDGE_CURVE ( 'NONE', #20034, #20000, #18980, .T. ) ;
#10407 = EDGE_CURVE ( 'NONE', #20071, #4844, #27723, .T. ) ;
#10408 = VERTEX_POINT ( 'NONE', #27442 ) ;
#10409 = ORIENTED_EDGE ( 'NONE', *, *, #19561, .T. ) ;
#10410 = LINE ( 'NONE', #1639, #12081 ) ;
#10411 = CARTESIAN_POINT ( 'NONE',  ( -290.0000000000001705, -220.0000000000000853, -59.99999999999986500 ) ) ;
#10412 = CARTESIAN_POINT ( 'NONE',  ( 8.117852850209656523, 141.5785587194356481, 12.99999999999999822 ) ) ;
#10413 = CARTESIAN_POINT ( 'NONE',  ( -230.8916957670046486, 130.8330661503599117, -5.000000000000002665 ) ) ;
#10414 = ADVANCED_FACE ( 'NONE', ( #14399 ), #25573, .F. ) ;
#10415 = CARTESIAN_POINT ( 'NONE',  ( 217.4999999999996305, 44.41075299063186321, -100.0000000000000142 ) ) ;
#10416 = DIRECTION ( 'NONE',  ( 0.000000000000000000, 0.000000000000000000, 1.000000000000000000 ) ) ;
#10417 = CARTESIAN_POINT ( 'NONE',  ( -226.6532499065050388, 62.99057865342161477, -8.245540320822751568 ) ) ;
#10418 = ORIENTED_EDGE ( 'NONE', *, *, #6350, .T. ) ;
#10419 = EDGE_CURVE ( 'NONE', #5065, #1356, #7782, .T. ) ;
#10420 = CARTESIAN_POINT ( 'NONE',  ( 1.250275373174975835, 1.249999999999999556, -7.480737022738206399 ) ) ;
#10421 = CARTESIAN_POINT ( 'NONE',  ( 158.0000000000014495, 66.01962454207041731, 45.00000000000000000 ) ) ;
#10422 = LINE ( 'NONE', #12593, #27904 ) ;
#10423 = FACE_OUTER_BOUND ( 'NONE', #16109, .T. ) ;
#10424 = AXIS2_PLACEMENT_3D ( 'NONE', #24754, #13559, #479 ) ;
#10425 = ORIENTED_EDGE ( 'NONE', *, *, #78, .T. ) ;
#10426 = DIRECTION ( 'NONE',  ( 1.000000000000000000, -0.000000000000000000, -0.000000000000000000 ) ) ;
#10427 = AXIS2_PLACEMENT_3D ( 'NONE', #1809, #19340, #19487 ) ;
#10428 = CARTESIAN_POINT ( 'NONE',  ( 33.10302365956999182, 221.6666220619077876, 15.00000000000000000 ) ) ;
#10429 = FACE_OUTER_BOUND ( 'NONE', #24002, .T. ) ;
#10430 = DIRECTION ( 'NONE',  ( -0.000000000000000000, -0.000000000000000000, -1.000000000000000000 ) ) ;
#10431 =( LENGTH_UNIT ( ) NAMED_UNIT ( * ) SI_UNIT ( .MILLI., .METRE. ) );
#10432 = CARTESIAN_POINT ( 'NONE',  ( -305.0000000000001137, -157.0000000000000284, -110.0000000000000284 ) ) ;
#10433 = VERTEX_POINT ( 'NONE', #27862 ) ;
#10434 = PLANE ( 'NONE',  #1976 ) ;
#10435 = VERTEX_POINT ( 'NONE', #16965 ) ;
#10436 = DIRECTION ( 'NONE',  ( -0.2066290158914672603, -0.9784193629480785193, 0.000000000000000000 ) ) ;
#10437 = ORIENTED_EDGE ( 'NONE', *, *, #19337, .F. ) ;
#10438 = ORIENTED_EDGE ( 'NONE', *, *, #12293, .T. ) ;
#10439 = PLANE ( 'NONE',  #24615 ) ;
#10440 = ADVANCED_FACE ( 'NONE', ( #16550 ), #25720, .F. ) ;
#10441 = VERTEX_POINT ( 'NONE', #3885 ) ;
#10442 = ORIENTED_EDGE ( 'NONE', *, *, #2546, .T. ) ;
#10443 = CARTESIAN_POINT ( 'NONE',  ( 113.0677398990922313, 214.9520504348329553, 97.20864094219221840 ) ) ;
#10444 = VECTOR ( 'NONE', #1706, 1000.000000000000227 ) ;
#10445 = CARTESIAN_POINT ( 'NONE',  ( 157.4999999999997442, 251.3484375938375024, 45.00000000000000000 ) ) ;
#10446 = PLANE ( 'NONE',  #7916 ) ;
#10447 = CARTESIAN_POINT ( 'NONE',  ( -160.5161435040798494, 120.3804527765386752, -22.28951900308573641 ) ) ;
#10448 = CARTESIAN_POINT ( 'NONE',  ( -200.0000000000000284, 0.000000000000000000, 25.00000000000000000 ) ) ;
#10449 = FACE_OUTER_BOUND ( 'NONE', #13989, .T. ) ;
#10450 = DIRECTION ( 'NONE',  ( -0.8018642810807398158, -0.5975062131282554700, 0.000000000000000000 ) ) ;
#10451 = CARTESIAN_POINT ( 'NONE',  ( -211.3659712544258298, 88.58350419819547028, -23.76025086788270357 ) ) ;
#10452 = CARTESIAN_POINT ( 'NONE',  ( 155.4185842870419947, 230.6339745962152392, 45.00000000000000000 ) ) ;
#10453 = CARTESIAN_POINT ( 'NONE',  ( 157.9999999999996874, 271.1575001501400379, -45.00000000000000000 ) ) ;
#10454 = DIRECTION ( 'NONE',  ( -0.000000000000000000, 0.000000000000000000, -1.000000000000000000 ) ) ;
#10455 = PLANE ( 'NONE',  #2677 ) ;
#10456 = FACE_OUTER_BOUND ( 'NONE', #8379, .T. ) ;
#10457 = ADVANCED_FACE ( 'NONE', ( #10504 ), #26570, .F. ) ;
#10458 = ORIENTED_EDGE ( 'NONE', *, *, #801, .F. ) ;
#10459 = ADVANCED_FACE ( 'NONE', ( #21850 ), #10791, .F. ) ;
#10460 = VECTOR ( 'NONE', #4434, 1000.000000000000000 ) ;
#10461 = VECTOR ( 'NONE', #24332, 1000.000000000000114 ) ;
#10462 = CARTESIAN_POINT ( 'NONE',  ( 118.0294372515228787, 204.4436508138956015, -45.00000000000000000 ) ) ;
#10463 = DIRECTION ( 'NONE',  ( 0.000000000000000000, -1.000000000000000000, 0.000000000000000000 ) ) ;
#10464 = ADVANCED_FACE ( 'NONE', ( #24151 ), #11074, .F. ) ;
#10465 = DIRECTION ( 'NONE',  ( 0.000000000000000000, 0.000000000000000000, -1.000000000000000000 ) ) ;
#10467 = ORIENTED_EDGE ( 'NONE', *, *, #9716, .F. ) ;
#10466 = ORIENTED_EDGE ( 'NONE', *, *, #1064, .F. ) ;
#10468 = CARTESIAN_POINT ( 'NONE',  ( 94.58250724493984762, 231.5191281348355119, -18.77838886173819688 ) ) ;
#10469 = ORIENTED_EDGE ( 'NONE', *, *, #17819, .T. ) ;
#10470 = EDGE_LOOP ( 'NONE', ( #24824, #7295, #16, #17356 ) ) ;
#10471 = ORIENTED_EDGE ( 'NONE', *, *, #22819, .T. ) ;
#10472 = VECTOR ( 'NONE', #19183, 1000.000000000000000 ) ;
#10473 = VERTEX_POINT ( 'NONE', #21983 ) ;
#10474 = VERTEX_POINT ( 'NONE', #26148 ) ;
#10475 = VERTEX_POINT ( 'NONE', #15252 ) ;
#10476 = DIRECTION ( 'NONE',  ( -0.8916010070299477119, -0.4528218681371110610, 0.000000000000000000 ) ) ;
#10477 = AXIS2_PLACEMENT_3D ( 'NONE', #1824, #10598, #6146 ) ;
#10478 = VECTOR ( 'NONE', #3409, 1000.000000000000000 ) ;
#10479 = DIRECTION ( 'NONE',  ( 0.4528218681383056610, -0.8916010070293409751, 0.000000000000000000 ) ) ;
#10480 = FACE_OUTER_BOUND ( 'NONE', #23821, .T. ) ;
#10481 = CARTESIAN_POINT ( 'NONE',  ( 232.4749999999995964, 133.0668745871126930, -42.86484227207692044 ) ) ;
#10482 = DIRECTION ( 'NONE',  ( 0.000000000000000000, 0.000000000000000000, 1.000000000000000000 ) ) ;
#10483 = EDGE_CURVE ( 'NONE', #22709, #25403, #17672, .T. ) ;
#10484 = DIRECTION ( 'NONE',  ( 0.4528218681372309096, -0.8916010070298868717, 0.000000000000000000 ) ) ;
#10485 = DIRECTION ( 'NONE',  ( 1.000000000000000000, 0.000000000000000000, 0.000000000000000000 ) ) ;
#10486 = ADVANCED_FACE ( 'NONE', ( #13 ), #24006, .F. ) ;
#10487 = ADVANCED_FACE ( 'NONE', ( #19971 ), #21704, .T. ) ;
#10489 = CARTESIAN_POINT ( 'NONE',  ( -68.57415822541635464, -23.01420295945612082, 100.0000000000000000 ) ) ;
#10488 = AXIS2_PLACEMENT_3D ( 'NONE', #1931, #5967, #21194 ) ;
#10490 = EDGE_CURVE ( 'NONE', #8066, #19372, #20743, .T. ) ;
#10491 = FACE_OUTER_BOUND ( 'NONE', #4622, .T. ) ;
#10492 = CARTESIAN_POINT ( 'NONE',  ( 217.4999999999996305, -5.589247009368136787, -100.0000000000000142 ) ) ;
#10493 = CARTESIAN_POINT ( 'NONE',  ( 187.4999999999996305, 133.0668745871126930, -36.86484227207694886 ) ) ;
#10494 = ORIENTED_EDGE ( 'NONE', *, *, #338, .T. ) ;
#10495 = DIRECTION ( 'NONE',  ( -0.8018642810807398158, -0.5975062131282554700, 0.000000000000000000 ) ) ;
#10496 = VECTOR ( 'NONE', #21471, 1000.000000000000000 ) ;
#10497 = PRODUCT_DEFINITION_SHAPE ( 'NONE', 'NONE',  #28400 ) ;
#10498 = CIRCLE ( 'NONE', #9102, 21.20097097723064294 ) ;
#10499 = CARTESIAN_POINT ( 'NONE',  ( -276.2002749566882471, -169.9725357324242907, -107.3290005716923901 ) ) ;
#10500 = EDGE_LOOP ( 'NONE', ( #11, #24495, #11145, #19374 ) ) ;
#10501 = ORIENTED_EDGE ( 'NONE', *, *, #16374, .T. ) ;
#10503 = ORIENTED_EDGE ( 'NONE', *, *, #20964, .F. ) ;
#10502 = VECTOR ( 'NONE', #19125, 1000.000000000000227 ) ;
#10504 = FACE_OUTER_BOUND ( 'NONE', #27249, .T. ) ;
#10505 = CARTESIAN_POINT ( 'NONE',  ( 157.9999999999997442, 249.0945000900840398, -45.00000000000000000 ) ) ;
#10506 = ORIENTED_EDGE ( 'NONE', *, *, #15132, .F. ) ;
#10507 = ORIENTED_EDGE ( 'NONE', *, *, #19550, .T. ) ;
#10508 = CARTESIAN_POINT ( 'NONE',  ( 82.68942924492586144, 110.0997128792066206, -99.99999999998921396 ) ) ;
#10509 = CARTESIAN_POINT ( 'NONE',  ( 101.0134428126900303, 235.9903891613491282, 23.57075532798359419 ) ) ;
#10510 = VECTOR ( 'NONE', #11132, 1000.000000000000227 ) ;
#10511 = CARTESIAN_POINT ( 'NONE',  ( -199.1255185106215322, 96.44980846386927453, -30.47972463551135647 ) ) ;
#10512 = CIRCLE ( 'NONE', #5937, 4.999999999999995559 ) ;
#10513 = ORIENTED_EDGE ( 'NONE', *, *, #1003, .T. ) ;
#10514 = CARTESIAN_POINT ( 'NONE',  ( -232.1897660433613453, 90.99944575719695194, 14.99999999999994849 ) ) ;
#10515 = EDGE_LOOP ( 'NONE', ( #20307, #13856, #23400, #20670, #19689, #5700 ) ) ;
#10516 = PLANE ( 'NONE',  #4269 ) ;
#10517 = EDGE_CURVE ( 'NONE', #27414, #3041, #302, .T. ) ;
#10518 = AXIS2_PLACEMENT_3D ( 'NONE', #22114, #23993, #24412 ) ;
#10519 = EDGE_CURVE ( 'NONE', #11930, #1493, #12966, .T. ) ;
#10520 = CARTESIAN_POINT ( 'NONE',  ( 0.000000000000000000, -18.01420295945611727, 95.00000000000000000 ) ) ;
#10521 = DIRECTION ( 'NONE',  ( 0.000000000000000000, 0.000000000000000000, -1.000000000000000000 ) ) ;
#10522 = EDGE_CURVE ( 'NONE', #16893, #1460, #28291, .T. ) ;
#10523 = CARTESIAN_POINT ( 'NONE',  ( 158.0000000000002558, 183.3818748873943889, -45.00000000000000000 ) ) ;
#10524 = VERTEX_POINT ( 'NONE', #6897 ) ;
#10525 = LINE ( 'NONE', #27465, #14608 ) ;
#10526 = EDGE_CURVE ( 'NONE', #15707, #20254, #18000, .T. ) ;
#10527 = PLANE ( 'NONE',  #7387 ) ;
#10528 = FACE_OUTER_BOUND ( 'NONE', #14996, .T. ) ;
#10529 = DIRECTION ( 'NONE',  ( -0.9506505318133544602, -0.3102637045530566295, 0.000000000000000000 ) ) ;
#10530 = ORIENTED_EDGE ( 'NONE', *, *, #4874, .F. ) ;
#10531 = CARTESIAN_POINT ( 'NONE',  ( 115.6411010564592061, 231.4666050640012998, 99.00000000000001421 ) ) ;
#10532 = CIRCLE ( 'NONE', #17868, 16.07743405327025243 ) ;
#10533 = DIRECTION ( 'NONE',  ( -0.000000000000000000, -0.000000000000000000, -1.000000000000000000 ) ) ;
#10534 = CARTESIAN_POINT ( 'NONE',  ( -206.8817896583512095, 90.46732954276036764, 26.12578640336038660 ) ) ;
#10535 = EDGE_LOOP ( 'NONE', ( #20367, #22627, #3425, #21551 ) ) ;
#10536 = VECTOR ( 'NONE', #6290, 1000.000000000000000 ) ;
#10537 = FACE_OUTER_BOUND ( 'NONE', #27722, .T. ) ;
#10538 = EDGE_LOOP ( 'NONE', ( #28293, #12680, #7389, #3776 ) ) ;
#10539 = AXIS2_PLACEMENT_3D ( 'NONE', #5087, #9267, #6812 ) ;
#10540 = LINE ( 'NONE', #16866, #22095 ) ;
#10541 = CARTESIAN_POINT ( 'NONE',  ( -162.3702703317349858, 119.5357951972386985, -23.00655219379951077 ) ) ;
#10542 = ORIENTED_EDGE ( 'NONE', *, *, #26928, .T. ) ;
#10543 = ORIENTED_EDGE ( 'NONE', *, *, #14749, .F. ) ;
#10544 = AXIS2_PLACEMENT_3D ( 'NONE', #15801, #9178, #17935 ) ;
#10545 = CARTESIAN_POINT ( 'NONE',  ( 157.4999999999998579, 153.5413123010633853, -45.00000000000000000 ) ) ;
#10546 = VERTEX_POINT ( 'NONE', #22273 ) ;
#10548 = EDGE_CURVE ( 'NONE', #20032, #21598, #10645, .T. ) ;
#10547 = ORIENTED_EDGE ( 'NONE', *, *, #18354, .T. ) ;
#10549 = ORIENTED_EDGE ( 'NONE', *, *, #28250, .T. ) ;
#10550 = DIRECTION ( 'NONE',  ( 1.000000000000000000, 0.000000000000000000, 1.921731041659628380E-16 ) ) ;
#10551 = EDGE_CURVE ( 'NONE', #26471, #12356, #4675, .T. ) ;
#10552 = AXIS2_PLACEMENT_3D ( 'NONE', #17756, #10878, #15620 ) ;
#10553 = PLANE ( 'NONE',  #2533 ) ;
#10554 = DIRECTION ( 'NONE',  ( 1.000000000000000000, 0.000000000000000000, 0.000000000000000000 ) ) ;
#10555 = DIRECTION ( 'NONE',  ( 0.4528218681378510801, 0.8916010070295719014, -0.000000000000000000 ) ) ;
#10556 = CARTESIAN_POINT ( 'NONE',  ( 118.3276951936840078, 204.8474345110799959, -99.88760442621965296 ) ) ;
#10557 = AXIS2_PLACEMENT_3D ( 'NONE', #27475, #16859, #16722 ) ;
#10558 = DIRECTION ( 'NONE',  ( 1.850371707708594316E-16, -1.000000000000000000, 0.000000000000000000 ) ) ;
#10559 = CARTESIAN_POINT ( 'NONE',  ( -236.2622743973891772, 68.21227378728583801, -5.744226217427297776 ) ) ;
#10560 = ORIENTED_EDGE ( 'NONE', *, *, #24363, .T. ) ;
#10561 = CARTESIAN_POINT ( 'NONE',  ( 0.6601832576049860846, 1.249999999999999556, -7.428391153593999263 ) ) ;
#10562 = DIRECTION ( 'NONE',  ( 1.000000000000000000, 0.000000000000000000, 0.000000000000000000 ) ) ;
#10563 = DIRECTION ( 'NONE',  ( 0.000000000000000000, -1.000000000000000000, 0.000000000000000000 ) ) ;
#10564 = CARTESIAN_POINT ( 'NONE',  ( 113.9142275403307565, 227.9126300401528908, -97.94883453769639914 ) ) ;
#10565 = ORIENTED_EDGE ( 'NONE', *, *, #4122, .F. ) ;
#10566 = FACE_OUTER_BOUND ( 'NONE', #40, .T. ) ;
#10567 = EDGE_CURVE ( 'NONE', #10408, #6088, #25448, .T. ) ;
#10568 = LINE ( 'NONE', #3420, #7487 ) ;
#10569 = CARTESIAN_POINT ( 'NONE',  ( -265.0337338324069947, -165.8360419968486781, 89.68688984748098392 ) ) ;
#10570 = DIRECTION ( 'NONE',  ( -0.2458199939946738577, -0.9693154958796741383, 0.000000000000000000 ) ) ;
#10571 =( NAMED_UNIT ( * ) SI_UNIT ( $, .STERADIAN. ) SOLID_ANGLE_UNIT ( ) );
#10572 = CARTESIAN_POINT ( 'NONE',  ( 158.0000000000003979, 170.8424998498591663, 45.00000000000000000 ) ) ;
#10573 = ORIENTED_EDGE ( 'NONE', *, *, #22869, .T. ) ;
#10574 = AXIS2_PLACEMENT_3D ( 'NONE', #6379, #20017, #19456 ) ;
#10575 = DIRECTION ( 'NONE',  ( -1.000000000000000000, 0.000000000000000000, 0.000000000000000000 ) ) ;
#10576 = VERTEX_POINT ( 'NONE', #15535 ) ;
#10577 = CARTESIAN_POINT ( 'NONE',  ( -71.37541315349507443, 240.0000000000000000, 5.000000000000002665 ) ) ;
#10578 = ORIENTED_EDGE ( 'NONE', *, *, #5032, .T. ) ;
#10579 = EDGE_CURVE ( 'NONE', #11112, #18951, #24282, .T. ) ;
#10580 = ORIENTED_EDGE ( 'NONE', *, *, #7231, .F. ) ;
#10581 = CARTESIAN_POINT ( 'NONE',  ( 157.4999999999998579, 120.9389372034718093, 45.00000000000000000 ) ) ;
#10582 = ORIENTED_EDGE ( 'NONE', *, *, #27601, .T. ) ;
#10583 = VECTOR ( 'NONE', #22224, 1000.000000000000000 ) ;
#10584 = ORIENTED_EDGE ( 'NONE', *, *, #7344, .F. ) ;
#10585 = ORIENTED_EDGE ( 'NONE', *, *, #5972, .F. ) ;
#10586 = CARTESIAN_POINT ( 'NONE',  ( 112.5004877479093324, 218.9596622748219090, 96.61493133138614553 ) ) ;
#10587 = CARTESIAN_POINT ( 'NONE',  ( -67.63633724927728963, 133.9262831905602127, -15.61889904559025943 ) ) ;
#10588 = DIRECTION ( 'NONE',  ( 1.000000000000000000, 1.321694076934710155E-16, 0.000000000000000000 ) ) ;
#10589 = ADVANCED_FACE ( 'NONE', ( #11662, #18252 ), #7478, .F. ) ;
#10590 = CARTESIAN_POINT ( 'NONE',  ( -148.2611599703591878, 125.4274327989001137, -17.54707401466952632 ) ) ;
#10591 = CARTESIAN_POINT ( 'NONE',  ( -272.1219990905822215, -170.1806730287380844, -93.00535902404892852 ) ) ;
#10592 = CARTESIAN_POINT ( 'NONE',  ( -268.6807300700924088, -170.5270201242149994, 88.72748730061762501 ) ) ;
#10593 = CARTESIAN_POINT ( 'NONE',  ( -226.3292334817031985, 89.73541284941354945, -15.87801632005360553 ) ) ;
#10594 = VECTOR ( 'NONE', #20947, 1000.000000000000114 ) ;
#10595 = CARTESIAN_POINT ( 'NONE',  ( 130.4856197046055684, 249.6586625914459034, -148.9571385985324525 ) ) ;
#10596 = CARTESIAN_POINT ( 'NONE',  ( -263.9672435214092729, -171.3034507378823719, -94.90501643659933961 ) ) ;
#10597 = LINE ( 'NONE', #8303, #15218 ) ;
#10598 = DIRECTION ( 'NONE',  ( 0.000000000000000000, 0.000000000000000000, 1.000000000000000000 ) ) ;
#10599 = CARTESIAN_POINT ( 'NONE',  ( 134.9999999999998579, 220.0000000000000284, -169.9999999999999716 ) ) ;
#10600 = ORIENTED_EDGE ( 'NONE', *, *, #1797, .F. ) ;
#10601 = ADVANCED_FACE ( 'NONE', ( #13812, #864 ), #16248, .T. ) ;
#10602 = CIRCLE ( 'NONE', #9228, 89.71075545852265520 ) ;
#10603 = ADVANCED_FACE ( 'NONE', ( #5311 ), #27004, .F. ) ;
#10604 = CARTESIAN_POINT ( 'NONE',  ( 157.9999999999998295, 231.0315000300280417, -45.00000000000000000 ) ) ;
#10605 = CARTESIAN_POINT ( 'NONE',  ( 145.6339745962156940, 199.5814157129578064, 45.00000000000000000 ) ) ;
#10606 = LINE ( 'NONE', #8310, #26214 ) ;
#10608 = VERTEX_POINT ( 'NONE', #22841 ) ;
#10607 = ORIENTED_EDGE ( 'NONE', *, *, #18351, .T. ) ;
#10609 = CARTESIAN_POINT ( 'NONE',  ( 100.2919976486446387, 242.8371140005963866, -14.10862752715507540 ) ) ;
#10610 = ORIENTED_EDGE ( 'NONE', *, *, #17205, .F. ) ;
#10611 = ORIENTED_EDGE ( 'NONE', *, *, #6465, .F. ) ;
#10612 = ADVANCED_FACE ( 'NONE', ( #18390 ), #20256, .T. ) ;
#10613 = ORIENTED_EDGE ( 'NONE', *, *, #20620, .T. ) ;
#10614 = VECTOR ( 'NONE', #26817, 1000.000000000000000 ) ;
#10615 = ORIENTED_EDGE ( 'NONE', *, *, #16188, .F. ) ;
#10616 = ORIENTED_EDGE ( 'NONE', *, *, #15714, .T. ) ;
#10617 = ORIENTED_EDGE ( 'NONE', *, *, #21572, .T. ) ;
#10618 = EDGE_CURVE ( 'NONE', #24084, #26943, #11938, .T. ) ;
#10619 = DIRECTION ( 'NONE',  ( 1.000000000000000000, 0.000000000000000000, 0.000000000000000000 ) ) ;
#10620 = EDGE_CURVE ( 'NONE', #23775, #20816, #15828, .T. ) ;
#10621 = VECTOR ( 'NONE', #20921, 1000.000000000000000 ) ;
#10622 = DIRECTION ( 'NONE',  ( 4.163336342344337027E-16, -1.000000000000000000, 1.387778780781445429E-16 ) ) ;
#10623 = EDGE_CURVE ( 'NONE', #14862, #13449, #26866, .T. ) ;
#10624 = DIRECTION ( 'NONE',  ( -0.8916010070296226386, 0.4528218681377511601, 0.000000000000000000 ) ) ;
#10625 = CARTESIAN_POINT ( 'NONE',  ( 187.4999999999996305, 258.6181251126050711, 1.387778780781445676E-14 ) ) ;
#10626 = LINE ( 'NONE', #6024, #6191 ) ;
#10627 = CARTESIAN_POINT ( 'NONE',  ( 158.0000000000015632, 57.98812451204224061, 45.00000000000000000 ) ) ;
#10628 = CARTESIAN_POINT ( 'NONE',  ( 157.4999999999996305, 286.4586876989355915, 45.00000000000000000 ) ) ;
#10629 = VECTOR ( 'NONE', #13429, 1000.000000000000000 ) ;
#10630 = DIRECTION ( 'NONE',  ( 1.000000000000000000, 0.000000000000000000, 0.000000000000000000 ) ) ;
#10631 = DIRECTION ( 'NONE',  ( 0.000000000000000000, 0.000000000000000000, 1.000000000000000000 ) ) ;
#10632 = ADVANCED_FACE ( 'NONE', ( #7336 ), #446, .T. ) ;
#10633 = LINE ( 'NONE', #15239, #6473 ) ;
#10634 = PLANE ( 'NONE',  #8375 ) ;
#10635 = VECTOR ( 'NONE', #26451, 1000.000000000000000 ) ;
#10636 = ORIENTED_EDGE ( 'NONE', *, *, #12021, .T. ) ;
#10637 = AXIS2_PLACEMENT_3D ( 'NONE', #25065, #2320, #14860 ) ;
#10638 = CARTESIAN_POINT ( 'NONE',  ( -188.7674184428050239, 104.2604349191509101, 32.38797585049563565 ) ) ;
#10639 = VECTOR ( 'NONE', #8561, 1000.000000000000227 ) ;
#10640 = CARTESIAN_POINT ( 'NONE',  ( -140.1213116003368668, 122.5384136796733827, 15.00000000000000000 ) ) ;
#10641 = ORIENTED_EDGE ( 'NONE', *, *, #22979, .T. ) ;
#10642 = APPLICATION_PROTOCOL_DEFINITION ( 'draft international standard', 'automotive_design', 1998, #4132 ) ;
#10643 = ORIENTED_EDGE ( 'NONE', *, *, #21419, .F. ) ;
#10644 = ORIENTED_EDGE ( 'NONE', *, *, #2436, .T. ) ;
#10645 = LINE ( 'NONE', #23862, #23971 ) ;
#10646 = CARTESIAN_POINT ( 'NONE',  ( -56.02075117275366978, 110.3042093914830559, -45.00000000000000000 ) ) ;
#10647 = ORIENTED_EDGE ( 'NONE', *, *, #21691, .F. ) ;
#10648 = VERTEX_POINT ( 'NONE', #26716 ) ;
#10649 = EDGE_CURVE ( 'NONE', #16763, #20178, #24715, .T. ) ;
#10650 = CARTESIAN_POINT ( 'NONE',  ( 82.91040908012101340, 80.00000000661717081, -100.0000000000000142 ) ) ;
#10651 = EDGE_CURVE ( 'NONE', #3632, #12751, #2727, .T. ) ;
#10652 = VECTOR ( 'NONE', #14663, 1000.000000000000114 ) ;
#10653 = CARTESIAN_POINT ( 'NONE',  ( 104.9999999999998579, 220.0000000000000284, -169.9999999999999716 ) ) ;
#10654 = CARTESIAN_POINT ( 'NONE',  ( -164.5329923790834528, 118.5024393687872504, -22.94354786372609212 ) ) ;
#10655 = ORIENTED_EDGE ( 'NONE', *, *, #16626, .T. ) ;
#10656 = CARTESIAN_POINT ( 'NONE',  ( -220.0435420340362214, 87.92826792072207809, 18.32348305083313278 ) ) ;
#10657 = ORIENTED_EDGE ( 'NONE', *, *, #12227, .F. ) ;
#10658 = DIRECTION ( 'NONE',  ( 0.4528218681382319422, -0.8916010070293783896, 0.000000000000000000 ) ) ;
#10659 = DIRECTION ( 'NONE',  ( 1.000000000000000000, -0.000000000000000000, -0.000000000000000000 ) ) ;
#10660 = PRESENTATION_LAYER_ASSIGNMENT (  '', '', ( #27159 ) ) ;
#10661 = CARTESIAN_POINT ( 'NONE',  ( 158.0000000000004263, 168.3346248423521274, 45.00000000000000000 ) ) ;
#10662 = CARTESIAN_POINT ( 'NONE',  ( 158.2656979116527793, 201.0591520573188973, -141.3400049877799063 ) ) ;
#10663 = DIRECTION ( 'NONE',  ( 0.000000000000000000, 0.000000000000000000, -1.000000000000000000 ) ) ;
#10664 = ORIENTED_EDGE ( 'NONE', *, *, #4761, .F. ) ;
#10665 = CARTESIAN_POINT ( 'NONE',  ( -295.0000000000001137, -165.0000000000000853, 60.00000000000002842 ) ) ;
#10666 = EDGE_CURVE ( 'NONE', #4885, #7590, #13960, .T. ) ;
#10667 = DIRECTION ( 'NONE',  ( 1.000000000000000000, 4.163336342344337027E-16, -0.000000000000000000 ) ) ;
#10668 = CARTESIAN_POINT ( 'NONE',  ( 158.0000000000006537, 143.7637497747887210, 45.00000000000000000 ) ) ;
#10669 = LINE ( 'NONE', #19429, #17625 ) ;
#10670 = ORIENTED_EDGE ( 'NONE', *, *, #14579, .F. ) ;
#10671 = VECTOR ( 'NONE', #837, 1000.000000000000114 ) ;
#10672 = LINE ( 'NONE', #17698, #21519 ) ;
#10673 = AXIS2_PLACEMENT_3D ( 'NONE', #15816, #24560, #1131 ) ;
#10674 = ADVANCED_FACE ( 'NONE', ( #727 ), #22706, .F. ) ;
#10675 = CARTESIAN_POINT ( 'NONE',  ( -181.6509543635144439, 108.9824211742952116, 30.31695520427327750 ) ) ;
#10676 = LINE ( 'NONE', #19433, #14241 ) ;
#10677 = LINE ( 'NONE', #21303, #14932 ) ;
#10678 = VERTEX_POINT ( 'NONE', #15770 ) ;
#10679 = DIRECTION ( 'NONE',  ( 0.000000000000000000, 0.000000000000000000, -1.000000000000000000 ) ) ;
#10680 = VECTOR ( 'NONE', #12375, 1000.000000000000000 ) ;
#10681 = ORIENTED_EDGE ( 'NONE', *, *, #13823, .F. ) ;
#10682 = VECTOR ( 'NONE', #23046, 1000.000000000000000 ) ;
#10683 = CARTESIAN_POINT ( 'NONE',  ( -210.0000000000000568, -220.0000000000000853, -110.0000000000000284 ) ) ;
#10684 = CARTESIAN_POINT ( 'NONE',  ( -182.9507880900968360, 107.8942440073746951, -31.71834794605663532 ) ) ;
#10685 = VERTEX_POINT ( 'NONE', #26952 ) ;
#10686 = ADVANCED_FACE ( 'NONE', ( #4824 ), #11607, .F. ) ;
#10687 = ORIENTED_EDGE ( 'NONE', *, *, #21180, .T. ) ;
#10688 = ADVANCED_FACE ( 'NONE', ( #4679 ), #2381, .T. ) ;
#10689 = LINE ( 'NONE', #6652, #7190 ) ;
#10690 = ORIENTED_EDGE ( 'NONE', *, *, #21641, .T. ) ;
#10691 = ADVANCED_FACE ( 'NONE', ( #19770 ), #2238, .F. ) ;
#10692 = ORIENTED_EDGE ( 'NONE', *, *, #18331, .T. ) ;
#10693 = EDGE_LOOP ( 'NONE', ( #27937, #15789, #24498, #6402 ) ) ;
#10694 = VECTOR ( 'NONE', #6936, 999.9999999999998863 ) ;
#10695 = DIRECTION ( 'NONE',  ( 0.8916010070293510781, -0.4528218681382856770, 0.000000000000000000 ) ) ;
#10696 = VECTOR ( 'NONE', #1755, 1000.000000000000227 ) ;
#10697 = DIRECTION ( 'NONE',  ( 0.7071067811865489050, 8.659560562354948882E-17, -0.7071067811865462405 ) ) ;
#10698 = CARTESIAN_POINT ( 'NONE',  ( 158.0000000000017053, 45.44874947450702507, -45.00000000000000000 ) ) ;
#10699 = CARTESIAN_POINT ( 'NONE',  ( 157.4999999999997726, 246.3326875788235384, 45.00000000000000000 ) ) ;
#10700 = AXIS2_PLACEMENT_3D ( 'NONE', #24809, #20207, #11612 ) ;
#10701 = AXIS2_PLACEMENT_3D ( 'NONE', #10722, #28221, #10155 ) ;
#10702 = FACE_OUTER_BOUND ( 'NONE', #10055, .T. ) ;
#10703 = CARTESIAN_POINT ( 'NONE',  ( -143.6428522700808230, 68.51688903468615877, 83.00000000000001421 ) ) ;
#10704 = CARTESIAN_POINT ( 'NONE',  ( -227.4113622183683106, 63.29489605847815881, -7.985794955240778314 ) ) ;
#10705 = ORIENTED_EDGE ( 'NONE', *, *, #7863, .T. ) ;
#10706 = DIRECTION ( 'NONE',  ( 0.000000000000000000, -1.000000000000000000, -1.214306433183764966E-16 ) ) ;
#10707 = CIRCLE ( 'NONE', #144, 10.71881775658151170 ) ;
#10708 = DIRECTION ( 'NONE',  ( -0.000000000000000000, -0.000000000000000000, -1.000000000000000000 ) ) ;
#10709 = DIRECTION ( 'NONE',  ( 0.000000000000000000, 1.000000000000000000, -1.224646799147353207E-16 ) ) ;
#10710 = CARTESIAN_POINT ( 'NONE',  ( 158.0000000000011653, 93.60624962464788723, -45.00000000000000000 ) ) ;
#10711 = ORIENTED_EDGE ( 'NONE', *, *, #19631, .T. ) ;
#10712 = LINE ( 'NONE', #3811, #11429 ) ;
#10713 = DIRECTION ( 'NONE',  ( 0.8916010070299470458, -0.4528218681371123377, 0.000000000000000000 ) ) ;
#10714 = DIRECTION ( 'NONE',  ( -0.000000000000000000, -0.000000000000000000, -1.000000000000000000 ) ) ;
#10715 = DIRECTION ( 'NONE',  ( 1.000000000000000000, 0.000000000000000000, 0.000000000000000000 ) ) ;
#10716 = CARTESIAN_POINT ( 'NONE',  ( 139.9999999999999147, 4.857225732735056078E-14, -100.0000000000000142 ) ) ;
#10717 = DIRECTION ( 'NONE',  ( -0.8660254037844363761, 0.5000000000000041078, -0.000000000000000000 ) ) ;
#10718 = ORIENTED_EDGE ( 'NONE', *, *, #16901, .F. ) ;
#10719 = VECTOR ( 'NONE', #2447, 1000.000000000000114 ) ;
#10720 = ADVANCED_FACE ( 'NONE', ( #8860 ), #22137, .T. ) ;
#10721 = CIRCLE ( 'NONE', #171, 30.49120955644046660 ) ;
#10722 = CARTESIAN_POINT ( 'NONE',  ( -210.0000000000000568, -157.0000000000000284, -105.0000000000000284 ) ) ;
#10723 = ORIENTED_EDGE ( 'NONE', *, *, #12618, .T. ) ;
#10724 = CARTESIAN_POINT ( 'NONE',  ( 158.0000000000013358, 80.55899957960563995, 45.00000000000000000 ) ) ;
#10725 = B_SPLINE_CURVE_WITH_KNOTS ( 'NONE', 3,
 ( #12792, #21536, #12373, #1849, #7900, #21112, #3720, #1429 ),
 .UNSPECIFIED., .F., .F.,
 ( 4, 2, 2, 4 ),
 ( 0.000000000000000000, 0.009823278049383234872, 0.01473491707407493558, 0.01964655609876663628 ),
 .UNSPECIFIED. ) ;
#10726 = ORIENTED_EDGE ( 'NONE', *, *, #259, .T. ) ;
#10727 = CIRCLE ( 'NONE', #18070, 49.99999999999998579 ) ;
#10728 = VERTEX_POINT ( 'NONE', #24095 ) ;
#10729 = LINE ( 'NONE', #8993, #15901 ) ;
#10730 = ADVANCED_FACE ( 'NONE', ( #6985 ), #6841, .T. ) ;
#10731 = EDGE_LOOP ( 'NONE', ( #28051, #16442, #19686, #4877 ) ) ;
#10732 = ORIENTED_EDGE ( 'NONE', *, *, #2120, .T. ) ;
#10733 = DIRECTION ( 'NONE',  ( -1.000000000000000000, 0.000000000000000000, 0.000000000000000000 ) ) ;
#10734 = DIRECTION ( 'NONE',  ( 0.000000000000000000, -1.000000000000000000, 0.000000000000000000 ) ) ;
#10735 = CARTESIAN_POINT ( 'NONE',  ( -212.3316009019935962, -218.3936534609811986, 93.13925850349481550 ) ) ;
#10736 = ADVANCED_FACE ( 'NONE', ( #20202 ), #13186, .F. ) ;
#10737 = CARTESIAN_POINT ( 'NONE',  ( 157.9999999999999147, 213.9842499849850697, 45.00000000000000000 ) ) ;
#10738 = FACE_OUTER_BOUND ( 'NONE', #5315, .T. ) ;
#10739 = CIRCLE ( 'NONE', #6608, 21.49999999999997868 ) ;
#10740 = CARTESIAN_POINT ( 'NONE',  ( -264.4418871519581558, -166.0055717401948527, -89.67623118319436060 ) ) ;
#10741 = CARTESIAN_POINT ( 'NONE',  ( -196.7918453702777128, 20.24192588826927164, 93.88690167569080813 ) ) ;
#10742 = CARTESIAN_POINT ( 'NONE',  ( -233.2943309833543140, 92.06151970357154823, -14.99999999999999645 ) ) ;
#10743 = CARTESIAN_POINT ( 'NONE',  ( 89.99999999999988631, 240.0000000000000284, -6.270166537926030514 ) ) ;
#10744 = CARTESIAN_POINT ( 'NONE',  ( -112.3221550338875687, 74.54464929955099706, 80.00000000000001421 ) ) ;
#10745 = CONICAL_SURFACE ( 'NONE', #5261, 6.025000000000002132, 0.7853981633971707232 ) ;
#10746 = CARTESIAN_POINT ( 'NONE',  ( 128.0812361363530272, 198.0425250404537394, -45.00000000000000000 ) ) ;
#10747 = DIRECTION ( 'NONE',  ( 1.000000000000000000, 0.000000000000000000, 0.000000000000000000 ) ) ;
#10748 = CARTESIAN_POINT ( 'NONE',  ( 319.9779125536060178, 113.2029523930392969, -145.0000000000000000 ) ) ;
#10749 = VERTEX_POINT ( 'NONE', #17906 ) ;
#10750 = CARTESIAN_POINT ( 'NONE',  ( 157.4999999999997442, 256.3641876088515232, -45.00000000000000000 ) ) ;
#10751 = DIRECTION ( 'NONE',  ( -0.8916010070298157064, -0.4528218681373708532, 0.000000000000000000 ) ) ;
#10752 = CARTESIAN_POINT ( 'NONE',  ( 107.3817056362660907, 208.2809019521421305, -149.7704424372629717 ) ) ;
#10753 = ORIENTED_EDGE ( 'NONE', *, *, #11531, .T. ) ;
#10754 = EDGE_CURVE ( 'NONE', #2647, #17690, #11022, .T. ) ;
#10755 = CARTESIAN_POINT ( 'NONE',  ( 96.18084660807248554, 232.2996298045119943, -19.72083291508440794 ) ) ;
#10756 = ORIENTED_EDGE ( 'NONE', *, *, #15298, .F. ) ;
#10757 = DIRECTION ( 'NONE',  ( 0.000000000000000000, 0.000000000000000000, -1.000000000000000000 ) ) ;
#10758 = ORIENTED_EDGE ( 'NONE', *, *, #22790, .T. ) ;
#10759 = ORIENTED_EDGE ( 'NONE', *, *, #17388, .F. ) ;
#10760 = VERTEX_POINT ( 'NONE', #6699 ) ;
#10761 = AXIS2_PLACEMENT_3D ( 'NONE', #21057, #7989, #9729 ) ;
#10762 = ORIENTED_EDGE ( 'NONE', *, *, #12650, .F. ) ;
#10763 = ORIENTED_EDGE ( 'NONE', *, *, #18926, .F. ) ;
#10764 = CARTESIAN_POINT ( 'NONE',  ( 158.0000000000006537, 141.2558747672816821, 45.00000000000000000 ) ) ;
#10765 = ADVANCED_FACE ( 'NONE', ( #15623 ), #528, .F. ) ;
#10766 = EDGE_CURVE ( 'NONE', #1235, #1528, #1488, .T. ) ;
#10767 = PLANE ( 'NONE',  #3646 ) ;
#10768 = DIRECTION ( 'NONE',  ( 0.8916010070293783896, -0.4528218681382319422, 0.000000000000000000 ) ) ;
#10769 = DIRECTION ( 'NONE',  ( 1.000000000000000000, 1.541976423090495880E-16, 0.000000000000000000 ) ) ;
#10770 = LINE ( 'NONE', #16426, #25044 ) ;
#10771 = CARTESIAN_POINT ( 'NONE',  ( -63.57415822541634043, -18.01420295945611727, 95.00000000000000000 ) ) ;
#10772 = DIRECTION ( 'NONE',  ( 0.9985600561963501320, 0.05364526231776645809, -0.000000000000000000 ) ) ;
#10773 = DIRECTION ( 'NONE',  ( 0.000000000000000000, 0.000000000000000000, 1.000000000000000000 ) ) ;
#10774 = AXIS2_PLACEMENT_3D ( 'NONE', #15085, #1710, #10482 ) ;
#10775 = EDGE_CURVE ( 'NONE', #20507, #14873, #14338, .T. ) ;
#10776 = ADVANCED_FACE ( 'NONE', ( #21930 ), #13464, .T. ) ;
#10777 = LINE ( 'NONE', #6457, #20575 ) ;
#10778 = FACE_OUTER_BOUND ( 'NONE', #8642, .T. ) ;
#10779 = DIRECTION ( 'NONE',  ( -0.000000000000000000, -0.000000000000000000, -1.000000000000000000 ) ) ;
#10780 = DIRECTION ( 'NONE',  ( 0.4528218681389001854, 0.8916010070290391054, -0.000000000000000000 ) ) ;
#10781 = AXIS2_PLACEMENT_3D ( 'NONE', #21587, #17139, #1897 ) ;
#10783 = ORIENTED_EDGE ( 'NONE', *, *, #19549, .T. ) ;
#10782 = ORIENTED_EDGE ( 'NONE', *, *, #18268, .F. ) ;
#10784 = CARTESIAN_POINT ( 'NONE',  ( -180.6173853931124711, 109.6284025331804628, 30.49881833197462910 ) ) ;
#10785 = CARTESIAN_POINT ( 'NONE',  ( 157.4999999999996305, 283.9508126914284958, 45.00000000000000000 ) ) ;
#10786 = ORIENTED_EDGE ( 'NONE', *, *, #4671, .F. ) ;
#10787 = APPLICATION_PROTOCOL_DEFINITION ( 'draft international standard', 'automotive_design', 1998, #1202 ) ;
#10788 = ADVANCED_FACE ( 'NONE', ( #677 ), #13324, .T. ) ;
#10789 = ORIENTED_EDGE ( 'NONE', *, *, #2934, .T. ) ;
#10790 = ORIENTED_EDGE ( 'NONE', *, *, #13135, .T. ) ;
#10791 = CYLINDRICAL_SURFACE ( 'NONE', #3779, 5.000000000000004441 ) ;
#10792 = PLANE ( 'NONE',  #28265 ) ;
#10793 = EDGE_LOOP ( 'NONE', ( #28357, #2084, #5791, #21157 ) ) ;
#10794 = VECTOR ( 'NONE', #8257, 1000.000000000000227 ) ;
#10795 = CIRCLE ( 'NONE', #25029, 29.99999999999998934 ) ;
#10796 = CARTESIAN_POINT ( 'NONE',  ( 93.07270601803662657, 112.9533406971499971, -74.06249999970600584 ) ) ;
#10797 = AXIS2_PLACEMENT_3D ( 'NONE', #5500, #22758, #1053 ) ;
#10798 = CARTESIAN_POINT ( 'NONE',  ( 158.0000000000001990, 188.3976249024084666, 45.00000000000000000 ) ) ;
#10799 = CARTESIAN_POINT ( 'NONE',  ( -173.5285038084994085, 113.8115965281807576, -27.00126897022071404 ) ) ;
#10800 = ORIENTED_EDGE ( 'NONE', *, *, #2567, .T. ) ;
#10801 = CARTESIAN_POINT ( 'NONE',  ( -222.5854910735133387, 88.44175340957714582, 17.19091714286218320 ) ) ;
#10802 = ORIENTED_EDGE ( 'NONE', *, *, #15962, .T. ) ;
#10803 = VECTOR ( 'NONE', #10958, 1000.000000000000000 ) ;
#10804 = CARTESIAN_POINT ( 'NONE',  ( -211.3305068427980871, -219.3267326664164614, 108.0785994798089433 ) ) ;
#10805 = DIRECTION ( 'NONE',  ( 1.000000000000000000, -0.000000000000000000, -0.000000000000000000 ) ) ;
#10806 = DIRECTION ( 'NONE',  ( 0.4528218681373320509, 0.8916010070298354684, -0.000000000000000000 ) ) ;
#10807 = DIRECTION ( 'NONE',  ( -0.000000000000000000, -0.000000000000000000, -1.000000000000000000 ) ) ;
#10808 = EDGE_LOOP ( 'NONE', ( #12395, #2932, #12956, #7374 ) ) ;
#10809 = CARTESIAN_POINT ( 'NONE',  ( 116.2405502098311558, 207.5638714341443176, 99.27293966533068215 ) ) ;
#10810 = AXIS2_PLACEMENT_3D ( 'NONE', #19730, #26333, #55 ) ;
#10811 = DIRECTION ( 'NONE',  ( 0.2066290158914390052, -0.9784193629480844034, 0.000000000000000000 ) ) ;
#10812 = DIRECTION ( 'NONE',  ( 0.000000000000000000, 0.000000000000000000, 1.000000000000000000 ) ) ;
#10813 = CARTESIAN_POINT ( 'NONE',  ( 158.0000000000010516, 103.6377496546760568, -45.00000000000000000 ) ) ;
#10814 = VECTOR ( 'NONE', #1370, 1000.000000000000000 ) ;
#10815 = VERTEX_POINT ( 'NONE', #7134 ) ;
#10816 = CARTESIAN_POINT ( 'NONE',  ( 157.4999999999998579, 118.4310621959647563, 45.00000000000000000 ) ) ;
#10817 = EDGE_CURVE ( 'NONE', #24310, #25171, #9442, .T. ) ;
#10818 = LINE ( 'NONE', #24307, #17598 ) ;
#10819 = CARTESIAN_POINT ( 'NONE',  ( 158.0000000000013642, 76.05112457209858690, 45.00000000000000000 ) ) ;
#10820 = DIRECTION ( 'NONE',  ( 1.000000000000000000, 1.321694076934710155E-16, -0.000000000000000000 ) ) ;
#10821 = EDGE_LOOP ( 'NONE', ( #26299, #3110 ) ) ;
#10822 = VECTOR ( 'NONE', #19874, 1000.000000000000000 ) ;
#10823 = ORIENTED_EDGE ( 'NONE', *, *, #14517, .F. ) ;
#10824 = CARTESIAN_POINT ( 'NONE',  ( 157.9999999999998010, 241.0630000600560550, 45.00000000000000000 ) ) ;
#10825 = CARTESIAN_POINT ( 'NONE',  ( -185.9585935723647765, 106.1799384177000718, -31.51628191568552140 ) ) ;
#10826 = ORIENTED_EDGE ( 'NONE', *, *, #19830, .F. ) ;
#10827 = EDGE_LOOP ( 'NONE', ( #16384, #24176, #992, #9099 ) ) ;
#10828 = DIRECTION ( 'NONE',  ( -0.8916010070293384215, 0.4528218681383106015, 0.000000000000000000 ) ) ;
#10829 = CARTESIAN_POINT ( 'NONE',  ( 158.0000000000007390, 135.7322497447605656, -45.00000000000000000 ) ) ;
#10830 = VECTOR ( 'NONE', #12200, 1000.000000000000000 ) ;
#10831 = ORIENTED_EDGE ( 'NONE', *, *, #24014, .F. ) ;
#10832 = ORIENTED_EDGE ( 'NONE', *, *, #23458, .T. ) ;
#10833 = VECTOR ( 'NONE', #13451, 999.9999999999998863 ) ;
#10834 = PLANE ( 'NONE',  #24451 ) ;
#10835 = EDGE_CURVE ( 'NONE', #23798, #9201, #24660, .T. ) ;
#10836 = DIRECTION ( 'NONE',  ( -0.000000000000000000, -0.000000000000000000, -1.000000000000000000 ) ) ;
#10837 = DIRECTION ( 'NONE',  ( 1.000000000000000000, -0.000000000000000000, -0.000000000000000000 ) ) ;
#10838 = LINE ( 'NONE', #200, #10342 ) ;
#10839 = AXIS2_PLACEMENT_3D ( 'NONE', #18577, #20870, #20724 ) ;
#10840 = LINE ( 'NONE', #11272, #1402 ) ;
#10841 = CARTESIAN_POINT ( 'NONE',  ( 158.0000000000011369, 96.11412463215494029, -45.00000000000000000 ) ) ;
#10842 = CARTESIAN_POINT ( 'NONE',  ( -226.0190876347137419, 72.67478414372106954, -17.85134081709557563 ) ) ;
#10843 = ORIENTED_EDGE ( 'NONE', *, *, #19407, .F. ) ;
#10844 = DIRECTION ( 'NONE',  ( 0.8018642810807398158, 0.5975062131282554700, -0.000000000000000000 ) ) ;
#10845 = EDGE_CURVE ( 'NONE', #11955, #8565, #14044, .T. ) ;
#10846 = CARTESIAN_POINT ( 'NONE',  ( -63.57415822541634043, 80.97823757117562593, 80.00000000000001421 ) ) ;
#10847 = DIRECTION ( 'NONE',  ( -0.000000000000000000, 0.000000000000000000, 1.000000000000000000 ) ) ;
#10848 = CARTESIAN_POINT ( 'NONE',  ( 112.7775258882242468, 223.5591602065040036, -96.91707758366551673 ) ) ;
#10849 = ORIENTED_EDGE ( 'NONE', *, *, #2655, .T. ) ;
#10850 = EDGE_CURVE ( 'NONE', #7120, #3880, #5538, .T. ) ;
#10851 = FACE_OUTER_BOUND ( 'NONE', #19900, .T. ) ;
#10852 = ADVANCED_FACE ( 'NONE', ( #5397 ), #20767, .F. ) ;
#10853 = ADVANCED_FACE ( 'NONE', ( #813 ), #18751, .F. ) ;
#10854 = LINE ( 'NONE', #1933, #23985 ) ;
#10855 = CARTESIAN_POINT ( 'NONE',  ( -76.25760768171835480, 221.6666220619077876, 15.00000000000000000 ) ) ;
#10856 = CARTESIAN_POINT ( 'NONE',  ( 158.0000000000011084, 98.62199963966197913, 45.00000000000000000 ) ) ;
#10857 = DIRECTION ( 'NONE',  ( -1.000000000000000000, 7.930164461608254523E-16, 0.000000000000000000 ) ) ;
#10858 = DIRECTION ( 'NONE',  ( 0.8314772792026874360, -0.5555587585212711232, 0.000000000000000000 ) ) ;
#10859 = ORIENTED_EDGE ( 'NONE', *, *, #27421, .T. ) ;
#10860 = AXIS2_PLACEMENT_3D ( 'NONE', #25073, #24932, #802 ) ;
#10861 = LINE ( 'NONE', #9274, #21688 ) ;
#10862 = ORIENTED_EDGE ( 'NONE', *, *, #25409, .T. ) ;
#10863 = CARTESIAN_POINT ( 'NONE',  ( 175.6862808370088089, 157.7720269260891826, 45.00000000000000000 ) ) ;
#10864 = VERTEX_POINT ( 'NONE', #20629 ) ;
#10865 = VECTOR ( 'NONE', #5259, 1000.000000000000000 ) ;
#10866 = VERTEX_POINT ( 'NONE', #23071 ) ;
#10867 = LINE ( 'NONE', #21782, #300 ) ;
#10868 = ORIENTED_EDGE ( 'NONE', *, *, #6390, .T. ) ;
#10869 = ORIENTED_EDGE ( 'NONE', *, *, #17914, .F. ) ;
#10870 = FACE_OUTER_BOUND ( 'NONE', #8881, .T. ) ;
#10871 = CARTESIAN_POINT ( 'NONE',  ( -52.82542805791850782, 131.8416355074880073, -16.11994505319805526 ) ) ;
#10872 = CARTESIAN_POINT ( 'NONE',  ( 147.3660254037845334, 200.5814157129577779, 45.00000000000000000 ) ) ;
#10873 = FACE_OUTER_BOUND ( 'NONE', #5771, .T. ) ;
#10874 = FACE_OUTER_BOUND ( 'NONE', #21859, .T. ) ;
#10875 = CONICAL_SURFACE ( 'NONE', #16838, 6.025000000000002132, 0.7853981633974482790 ) ;
#10876 = EDGE_CURVE ( 'NONE', #5381, #6186, #23210, .T. ) ;
#10877 = CIRCLE ( 'NONE', #23728, 10.71881775658151170 ) ;
#10878 = DIRECTION ( 'NONE',  ( -0.000000000000000000, -0.000000000000000000, 1.000000000000000000 ) ) ;
#10879 = EDGE_CURVE ( 'NONE', #16770, #5280, #27228, .T. ) ;
#10880 = DIRECTION ( 'NONE',  ( -0.000000000000000000, 1.000000000000000000, -1.387778780781445429E-16 ) ) ;
#10881 = CARTESIAN_POINT ( 'NONE',  ( -211.8454146708414498, 88.46767467987882583, -21.92683318774069079 ) ) ;
#10882 = CARTESIAN_POINT ( 'NONE',  ( 0.3651377028998192276, -1.249999999999998890, -7.402212548648222423 ) ) ;
#10883 = DIRECTION ( 'NONE',  ( 0.000000000000000000, 0.000000000000000000, -1.000000000000000000 ) ) ;
#10884 = DIRECTION ( 'NONE',  ( -1.000000000000000000, 0.000000000000000000, 0.000000000000000000 ) ) ;
#10885 = CARTESIAN_POINT ( 'NONE',  ( 112.5248869502488134, 224.9869122110685282, -45.00000000000000000 ) ) ;
#10886 = DIRECTION ( 'NONE',  ( 0.5000000000000039968, 0.8660254037844364872, 0.000000000000000000 ) ) ;
#10887 = ORIENTED_EDGE ( 'NONE', *, *, #16934, .F. ) ;
#10888 = FACE_OUTER_BOUND ( 'NONE', #26318, .T. ) ;
#10889 = EDGE_CURVE ( 'NONE', #15333, #9950, #598, .T. ) ;
#10890 = LINE ( 'NONE', #4274, #3640 ) ;
#10891 = DIRECTION ( 'NONE',  ( 1.850371707708594316E-16, -1.000000000000000000, 0.000000000000000000 ) ) ;
#10892 = CARTESIAN_POINT ( 'NONE',  ( 33.10302365956999182, 203.2034914284457159, 12.99999999999999822 ) ) ;
#10893 = VERTEX_POINT ( 'NONE', #5683 ) ;
#10894 = EDGE_CURVE ( 'NONE', #20219, #14406, #22621, .T. ) ;
#10895 = CARTESIAN_POINT ( 'NONE',  ( 91.17299970895513184, 230.3777436784973816, -17.14176051628210828 ) ) ;
#10896 = ORIENTED_EDGE ( 'NONE', *, *, #18498, .T. ) ;
#10897 = CARTESIAN_POINT ( 'NONE',  ( -13.80176969007178478, 130.8724268707720171, -14.97137485413120395 ) ) ;
#10898 = ORIENTED_EDGE ( 'NONE', *, *, #27498, .T. ) ;
#10899 = AXIS2_PLACEMENT_3D ( 'NONE', #9745, #16220, #14067 ) ;
#10900 = ORIENTED_EDGE ( 'NONE', *, *, #7515, .F. ) ;
#10901 = ORIENTED_EDGE ( 'NONE', *, *, #4585, .F. ) ;
#10902 = ORIENTED_EDGE ( 'NONE', *, *, #1018, .T. ) ;
#10903 = VERTEX_POINT ( 'NONE', #9856 ) ;
#10904 = DIRECTION ( 'NONE',  ( 0.4528218681382713551, 0.8916010070293584056, -0.000000000000000000 ) ) ;
#10905 = FACE_OUTER_BOUND ( 'NONE', #16484, .T. ) ;
#10906 = LINE ( 'NONE', #4145, #9349 ) ;
#10907 = CARTESIAN_POINT ( 'NONE',  ( -206.2579005266799186, 60.21847207785817346, 20.52143262683453528 ) ) ;
#10909 = CONICAL_SURFACE ( 'NONE', #7696, 5.999999999999977796, 1.029744258676652091 ) ;
#10908 = CARTESIAN_POINT ( 'NONE',  ( 157.4999999999998295, 226.2696875187675118, 45.00000000000000000 ) ) ;
#10910 = EDGE_CURVE ( 'NONE', #5551, #14300, #15285, .T. ) ;
#10911 = DIRECTION ( 'NONE',  ( -0.000000000000000000, 1.000000000000000000, 1.214306433183764966E-16 ) ) ;
#10912 = DIRECTION ( 'NONE',  ( 2.602085213965210642E-16, -1.000000000000000000, 0.000000000000000000 ) ) ;
#10913 = LINE ( 'NONE', #24264, #237 ) ;
#10914 = LINE ( 'NONE', #6508, #2659 ) ;
#10915 = DIRECTION ( 'NONE',  ( -0.000000000000000000, 0.000000000000000000, 1.000000000000000000 ) ) ;
#10916 = CARTESIAN_POINT ( 'NONE',  ( -209.0137874940113818, 69.92142720080950369, 37.51845061662766057 ) ) ;
#10917 = CARTESIAN_POINT ( 'NONE',  ( -71.37541315349507443, 150.2892445414773590, -5.000000000000004441 ) ) ;
#10918 = FACE_OUTER_BOUND ( 'NONE', #20753, .T. ) ;
#10920 = ORIENTED_EDGE ( 'NONE', *, *, #20149, .T. ) ;
#10919 = ORIENTED_EDGE ( 'NONE', *, *, #10618, .T. ) ;
#10921 = CARTESIAN_POINT ( 'NONE',  ( -184.2222344732742556, 107.3439714424985993, 31.61955583114170309 ) ) ;
#10922 = EDGE_CURVE ( 'NONE', #26795, #6015, #14312, .T. ) ;
#10923 = ADVANCED_FACE ( 'NONE', ( #27502 ), #11625, .F. ) ;
#10924 = LINE ( 'NONE', #4310, #19060 ) ;
#10925 = ORIENTED_EDGE ( 'NONE', *, *, #2663, .T. ) ;
#10926 = PRODUCT_CONTEXT ( 'NONE', #10020, 'mechanical' ) ;
#10927 = EDGE_CURVE ( 'NONE', #7126, #15348, #15735, .T. ) ;
#10928 = ORIENTED_EDGE ( 'NONE', *, *, #8545, .F. ) ;
#10929 = VERTEX_POINT ( 'NONE', #16605 ) ;
#10930 = AXIS2_PLACEMENT_3D ( 'NONE', #20835, #18678, #27425 ) ;
#10931 = DIRECTION ( 'NONE',  ( 0.4528218681374919785, 0.8916010070297542001, -0.000000000000000000 ) ) ;
#10932 = DIRECTION ( 'NONE',  ( 1.000000000000000000, -0.000000000000000000, -0.000000000000000000 ) ) ;
#10933 = VECTOR ( 'NONE', #172, 1000.000000000000227 ) ;
#10934 = ORIENTED_EDGE ( 'NONE', *, *, #27526, .T. ) ;
#10935 = EDGE_CURVE ( 'NONE', #9674, #16172, #14455, .T. ) ;
#10936 = CARTESIAN_POINT ( 'NONE',  ( 109.9999999999999147, 137.0808454112663810, -89.99999999930710715 ) ) ;
#10937 = ADVANCED_FACE ( 'NONE', ( #24804 ), #13905, .F. ) ;
#10938 =( REPRESENTATION_RELATIONSHIP ('NONE','NONE', #11963, #24038 ) REPRESENTATION_RELATIONSHIP_WITH_TRANSFORMATION ( #15102 )SHAPE_REPRESENTATION_RELATIONSHIP( ) );
#10939 = CARTESIAN_POINT ( 'NONE',  ( 109.9999999999999147, 140.0000000000000000, 100.0000000000000142 ) ) ;
#10940 = ORIENTED_EDGE ( 'NONE', *, *, #28105, .T. ) ;
#10941 = CARTESIAN_POINT ( 'NONE',  ( -211.3652297710211201, 88.58433376602883413, 23.76089942878013161 ) ) ;
#10942 = ORIENTED_EDGE ( 'NONE', *, *, #16608, .F. ) ;
#10943 = CARTESIAN_POINT ( 'NONE',  ( -213.0597602322720832, -217.1208202143830306, 105.3784789975249794 ) ) ;
#10944 = VECTOR ( 'NONE', #20838, 1000.000000000000000 ) ;
#10945 = CARTESIAN_POINT ( 'NONE',  ( 157.4999999999996874, 271.4114376538935289, -45.00000000000000000 ) ) ;
#10946 = CARTESIAN_POINT ( 'NONE',  ( 109.9999999999999289, -90.00000000000001421, -70.00000000000001421 ) ) ;
#10947 = ORIENTED_EDGE ( 'NONE', *, *, #17974, .T. ) ;
#10948 = DIRECTION ( 'NONE',  ( -0.8660254037844432595, -0.4999999999999920064, 0.000000000000000000 ) ) ;
#10949 = VECTOR ( 'NONE', #16639, 1000.000000000000114 ) ;
#10950 = CARTESIAN_POINT ( 'NONE',  ( 139.9999999999999716, -100.0000000000000000, 100.0000000000000142 ) ) ;
#10951 = DIRECTION ( 'NONE',  ( -2.775557561562887407E-16, -3.668437989309015850E-32, -1.000000000000000000 ) ) ;
#10952 = CYLINDRICAL_SURFACE ( 'NONE', #2947, 100.0000000000000284 ) ;
#10953 = ORIENTED_EDGE ( 'NONE', *, *, #7052, .F. ) ;
#10954 = CARTESIAN_POINT ( 'NONE',  ( 157.4751130497510303, 215.0130877889310455, 45.00000000000000000 ) ) ;
#10955 = ADVANCED_FACE ( 'NONE', ( #18480 ), #7569, .F. ) ;
#10956 = EDGE_CURVE ( 'NONE', #17690, #15187, #3234, .T. ) ;
#10957 = CARTESIAN_POINT ( 'NONE',  ( 158.0000000000009663, 113.1613746771971876, 45.00000000000000000 ) ) ;
#10958 = DIRECTION ( 'NONE',  ( 1.000000000000000000, 1.530283246943720875E-16, -0.000000000000000000 ) ) ;
#10959 = ORIENTED_EDGE ( 'NONE', *, *, #8794, .F. ) ;
#10960 = SHAPE_REPRESENTATION_RELATIONSHIP ( 'NONE' , 'NONE' ,  #3128, #9885 ) ;
#10961 = VERTEX_POINT ( 'NONE', #5959 ) ;
#10962 = DIRECTION ( 'NONE',  ( -0.8916010070293409751, -0.4528218681383056610, 0.000000000000000000 ) ) ;
#10963 = VECTOR ( 'NONE', #27849, 1000.000000000000000 ) ;
#10964 = CARTESIAN_POINT ( 'NONE',  ( -191.3994286864096637, 102.3862160203461400, -32.47203723438894940 ) ) ;
#10965 = EDGE_LOOP ( 'NONE', ( #20710, #11573, #8111, #14319 ) ) ;
#10967 = ORIENTED_EDGE ( 'NONE', *, *, #22948, .F. ) ;
#10966 = ADVANCED_FACE ( 'NONE', ( #10280 ), #8086, .T. ) ;
#10968 = CARTESIAN_POINT ( 'NONE',  ( -524.0002167759885197, -169.4627935898112696, 0.000000000000000000 ) ) ;
#10969 = CONICAL_SURFACE ( 'NONE', #14182, 6.025000000000002132, 0.7853981633974482790 ) ;
#10970 = PRODUCT_DEFINITION_SHAPE ( 'NONE', 'NONE',  #28401 ) ;
#10971 = CARTESIAN_POINT ( 'NONE',  ( 157.9999999999998010, 233.5393750375350237, -45.00000000000000000 ) ) ;
#10972 = EDGE_LOOP ( 'NONE', ( #26833, #657, #17286, #2358 ) ) ;
#10973 = ORIENTED_EDGE ( 'NONE', *, *, #14841, .T. ) ;
#10974 = EDGE_CURVE ( 'NONE', #20823, #9382, #21685, .T. ) ;
#10975 = CARTESIAN_POINT ( 'NONE',  ( -43.02437977270766822, 129.7200458115292747, 16.81627168235289815 ) ) ;
#10977 = EDGE_CURVE ( 'NONE', #17587, #18428, #20689, .T. ) ;
#10976 = VECTOR ( 'NONE', #17970, 1000.000000000000000 ) ;
#10978 = CARTESIAN_POINT ( 'NONE',  ( -200.0000000000000284, -91.18033988749901653, -21.20097097723064294 ) ) ;
#10979 = EDGE_CURVE ( 'NONE', #27519, #2485, #10067, .T. ) ;
#10980 = PLANE ( 'NONE',  #24067 ) ;
#10981 = LINE ( 'NONE', #22032, #26410 ) ;
#10982 = CARTESIAN_POINT ( 'NONE',  ( 157.4999999999998579, 143.5098122710352015, -45.00000000000000000 ) ) ;
#10983 = CARTESIAN_POINT ( 'NONE',  ( 157.4999999999996305, 283.9508126914284958, -45.00000000000000000 ) ) ;
#10984 = DIRECTION ( 'NONE',  ( 0.4528218681383305855, -0.8916010070293283185, 0.000000000000000000 ) ) ;
#10985 = ORIENTED_EDGE ( 'NONE', *, *, #11177, .T. ) ;
#10986 = AXIS2_PLACEMENT_3D ( 'NONE', #4232, #26205, #13022 ) ;
#10987 = CARTESIAN_POINT ( 'NONE',  ( 167.4999999999996589, -5.589247009368157215, 84.99999999999995737 ) ) ;
#10988 = VECTOR ( 'NONE', #23514, 1000.000000000000114 ) ;
#10989 = PLANE ( 'NONE',  #26228 ) ;
#10990 = CARTESIAN_POINT ( 'NONE',  ( 158.0000000000009095, 120.6849996997183183, 45.00000000000000000 ) ) ;
#10991 = CARTESIAN_POINT ( 'NONE',  ( 40.99999999999999289, 0.000000000000000000, 0.000000000000000000 ) ) ;
#10992 = ORIENTED_EDGE ( 'NONE', *, *, #1668, .T. ) ;
#10993 = FACE_OUTER_BOUND ( 'NONE', #1182, .T. ) ;
#10994 = VECTOR ( 'NONE', #11650, 1000.000000000000000 ) ;
#10995 = ORIENTED_EDGE ( 'NONE', *, *, #18247, .T. ) ;
#10996 = LINE ( 'NONE', #16580, #14375 ) ;
#10997 = CARTESIAN_POINT ( 'NONE',  ( -260.0000000000001137, -220.0000000000000853, -89.99999999999985789 ) ) ;
#10998 = CARTESIAN_POINT ( 'NONE',  ( 157.4999999999998579, 220.0000000000000284, 99.00000000000001421 ) ) ;
#10999 = LINE ( 'NONE', #13164, #23021 ) ;
#11000 = CARTESIAN_POINT ( 'NONE',  ( 232.4999999999996305, 133.0668745871126930, 42.86484227207692044 ) ) ;
#11001 = EDGE_CURVE ( 'NONE', #25311, #24933, #21114, .T. ) ;
#11002 = ORIENTED_EDGE ( 'NONE', *, *, #20379, .T. ) ;
#11003 = VECTOR ( 'NONE', #9035, 1000.000000000000000 ) ;
#11004 = CARTESIAN_POINT ( 'NONE',  ( 79.99999999999991473, 80.00000000000001421, -100.0000000000000142 ) ) ;
#11005 = ORIENTED_EDGE ( 'NONE', *, *, #18565, .T. ) ;
#11006 = DIRECTION ( 'NONE',  ( 0.000000000000000000, 0.000000000000000000, 1.000000000000000000 ) ) ;
#11007 = ORIENTED_EDGE ( 'NONE', *, *, #20546, .T. ) ;
#11008 = ORIENTED_EDGE ( 'NONE', *, *, #24681, .T. ) ;
#11009 = CARTESIAN_POINT ( 'NONE',  ( 158.0000000000014779, 63.51174953456337136, 45.00000000000000000 ) ) ;
#11010 = VECTOR ( 'NONE', #2233, 1000.000000000000114 ) ;
#11011 = ORIENTED_EDGE ( 'NONE', *, *, #6899, .T. ) ;
#11012 = VERTEX_POINT ( 'NONE', #10207 ) ;
#11013 = CARTESIAN_POINT ( 'NONE',  ( -279.3160071107327553, -512.7211954420570237, -9.184850993605147944E-16 ) ) ;
#11014 = CARTESIAN_POINT ( 'NONE',  ( 104.4928295061213248, 246.1605864358052713, 20.56267333364200667 ) ) ;
#11015 = EDGE_CURVE ( 'NONE', #10405, #4982, #16674, .T. ) ;
#11016 = AXIS2_PLACEMENT_3D ( 'NONE', #4975, #6994, #13912 ) ;
#11017 = EDGE_CURVE ( 'NONE', #5089, #12678, #25426, .T. ) ;
#11018 = PLANE ( 'NONE',  #5737 ) ;
#11019 = DIRECTION ( 'NONE',  ( 1.000000000000000000, 0.000000000000000000, 0.000000000000000000 ) ) ;
#11020 = FACE_OUTER_BOUND ( 'NONE', #17077, .T. ) ;
#11021 = CARTESIAN_POINT ( 'NONE',  ( 158.0000000000003695, 173.3503748573662051, 45.00000000000000000 ) ) ;
#11022 = LINE ( 'NONE', #22073, #23047 ) ;
#11023 = DIRECTION ( 'NONE',  ( -0.000000000000000000, 0.000000000000000000, -1.000000000000000000 ) ) ;
#11024 = DIRECTION ( 'NONE',  ( 0.000000000000000000, 0.000000000000000000, -1.000000000000000000 ) ) ;
#11025 = LINE ( 'NONE', #21933, #22555 ) ;
#11026 = CARTESIAN_POINT ( 'NONE',  ( -71.37541315349507443, 240.0000000000000000, 15.00000000000000000 ) ) ;
#11027 = CARTESIAN_POINT ( 'NONE',  ( 158.0000000000000000, 206.4606249624626457, 45.00000000000000000 ) ) ;
#11028 = EDGE_LOOP ( 'NONE', ( #22305, #3249, #8174, #16239 ) ) ;
#11029 = CARTESIAN_POINT ( 'NONE',  ( -175.0000000000000000, -173.6051637141655419, 70.00000000000002842 ) ) ;
#11030 = VECTOR ( 'NONE', #23806, 1000.000000000000000 ) ;
#11031 = DIRECTION ( 'NONE',  ( 1.000000000000000000, 0.000000000000000000, 0.000000000000000000 ) ) ;
#11032 = CARTESIAN_POINT ( 'NONE',  ( 157.9999999999998010, 239.0630000600560550, 45.00000000000000000 ) ) ;
#11033 = CARTESIAN_POINT ( 'NONE',  ( 107.8677974404447752, 207.1985680636095424, -139.5328759577091660 ) ) ;
#11034 = ORIENTED_EDGE ( 'NONE', *, *, #17136, .F. ) ;
#11035 = AXIS2_PLACEMENT_3D ( 'NONE', #21302, #8377, #28033 ) ;
#11036 = DIRECTION ( 'NONE',  ( -0.6681556583950049033, 0.7440215159219103480, 0.000000000000000000 ) ) ;
#11037 = EDGE_LOOP ( 'NONE', ( #5083, #2758, #8207, #26384 ) ) ;
#11038 = CARTESIAN_POINT ( 'NONE',  ( -5.362417151017317529, 133.6996939015124326, -14.05114881981127972 ) ) ;
#11039 = VERTEX_POINT ( 'NONE', #20836 ) ;
#11040 = ORIENTED_EDGE ( 'NONE', *, *, #3205, .T. ) ;
#11041 = ORIENTED_EDGE ( 'NONE', *, *, #24397, .T. ) ;
#11042 = VERTEX_POINT ( 'NONE', #7631 ) ;
#11043 = ORIENTED_EDGE ( 'NONE', *, *, #25133, .F. ) ;
#11044 = DIRECTION ( 'NONE',  ( 1.000000000000000000, 0.000000000000000000, 0.000000000000000000 ) ) ;
#11045 = EDGE_CURVE ( 'NONE', #26706, #19122, #18964, .T. ) ;
#11046 = CIRCLE ( 'NONE', #7380, 5.000000000000004441 ) ;
#11047 = EDGE_CURVE ( 'NONE', #21857, #12635, #2884, .T. ) ;
#11048 = DIRECTION ( 'NONE',  ( 0.8916010070297948342, -0.4528218681374120425, 0.000000000000000000 ) ) ;
#11049 = CARTESIAN_POINT ( 'NONE',  ( 134.9999999999998579, 220.0000000000000284, -99.00000000000001421 ) ) ;
#11050 = CIRCLE ( 'NONE', #27104, 58.59270260175150469 ) ;
#11051 = CARTESIAN_POINT ( 'NONE',  ( -203.1048999768048589, 60.64878749907337152, 23.79654850876809036 ) ) ;
#11052 = LINE ( 'NONE', #23983, #6449 ) ;
#11053 = CARTESIAN_POINT ( 'NONE',  ( 158.0000000000007674, 131.2243747372535267, 45.00000000000000000 ) ) ;
#11054 = CARTESIAN_POINT ( 'NONE',  ( -210.7172313291012529, 103.7585653882801182, -5.000000000000004441 ) ) ;
#11055 = CARTESIAN_POINT ( 'NONE',  ( 157.4999999999996874, 266.3956876388795649, 45.00000000000000000 ) ) ;
#11056 = FACE_OUTER_BOUND ( 'NONE', #4449, .T. ) ;
#11057 = CARTESIAN_POINT ( 'NONE',  ( -235.6744655116503964, 80.57819178535525850, -15.03015451089642873 ) ) ;
#11058 = CARTESIAN_POINT ( 'NONE',  ( -26.97244491501115604, 127.9665432412413537, 17.51913689374569927 ) ) ;
#11059 = CARTESIAN_POINT ( 'NONE',  ( -260.0000000000001137, -152.0000000000000284, -59.99999999999986500 ) ) ;
#11060 = VECTOR ( 'NONE', #14235, 1000.000000000000227 ) ;
#11061 = CARTESIAN_POINT ( 'NONE',  ( 157.9999999999996874, 264.1417501351260171, -45.00000000000000000 ) ) ;
#11062 = CARTESIAN_POINT ( 'NONE',  ( 217.4999999999996305, 494.4107529906318632, 100.0000000000000142 ) ) ;
#11064 = ORIENTED_EDGE ( 'NONE', *, *, #14326, .F. ) ;
#11063 = ORIENTED_EDGE ( 'NONE', *, *, #8578, .T. ) ;
#11065 = CARTESIAN_POINT ( 'NONE',  ( -186.0333716493514089, 106.1453078209526950, 32.04635124596575224 ) ) ;
#11066 = AXIS2_PLACEMENT_3D ( 'NONE', #22252, #4328, #2563 ) ;
#11067 = CARTESIAN_POINT ( 'NONE',  ( -204.2386885291766134, 92.18108640773468210, -28.15472916265547809 ) ) ;
#11068 = EDGE_LOOP ( 'NONE', ( #2910, #27618, #7722, #5705 ) ) ;
#11069 = EDGE_CURVE ( 'NONE', #14725, #5248, #6629, .T. ) ;
#11070 = VERTEX_POINT ( 'NONE', #19387 ) ;
#11071 = ORIENTED_EDGE ( 'NONE', *, *, #6593, .F. ) ;
#11072 = AXIS2_PLACEMENT_3D ( 'NONE', #25015, #1299, #24874 ) ;
#11073 = EDGE_CURVE ( 'NONE', #25416, #223, #15380, .T. ) ;
#11074 = PLANE ( 'NONE',  #2399 ) ;
#11075 = CARTESIAN_POINT ( 'NONE',  ( -144.2277858775206028, 125.7111241703296969, 18.60581271085799315 ) ) ;
#11076 = VERTEX_POINT ( 'NONE', #12794 ) ;
#11077 = CARTESIAN_POINT ( 'NONE',  ( 85.37729192593057803, 80.27798593821322015, -100.0000000000000142 ) ) ;
#11078 = ADVANCED_FACE ( 'NONE', ( #23846 ), #27991, .F. ) ;
#11079 = CARTESIAN_POINT ( 'NONE',  ( 157.4999999999995168, 208.7145624662163925, -45.00000000000000000 ) ) ;
#11080 = ORIENTED_EDGE ( 'NONE', *, *, #2331, .T. ) ;
#11081 = CARTESIAN_POINT ( 'NONE',  ( -226.4313904733368474, 87.63842543593344203, 16.09009735459598645 ) ) ;
#11082 = DIRECTION ( 'NONE',  ( -1.000000000000000000, 0.000000000000000000, 0.000000000000000000 ) ) ;
#11083 = ADVANCED_FACE ( 'NONE', ( #23991 ), #4150, .F. ) ;
#11084 = AXIS2_PLACEMENT_3D ( 'NONE', #27818, #28101, #21367 ) ;
#11085 = DIRECTION ( 'NONE',  ( -1.000000000000000000, 0.000000000000000000, -9.251858538542972814E-17 ) ) ;
#11086 = CARTESIAN_POINT ( 'NONE',  ( 157.8121286602244027, 200.5163485565246049, -142.5205423047663373 ) ) ;
#11087 = AXIS2_PLACEMENT_3D ( 'NONE', #25478, #27760, #12000 ) ;
#11088 = AXIS2_PLACEMENT_3D ( 'NONE', #14924, #27826, #6005 ) ;
#11089 = EDGE_LOOP ( 'NONE', ( #26182, #22530, #14614, #13601 ) ) ;
#11090 = DIRECTION ( 'NONE',  ( 0.000000000000000000, 0.5150380749100563760, 0.8571673007021110013 ) ) ;
#11091 = CARTESIAN_POINT ( 'NONE',  ( -219.9082363642798441, 137.1815813412079308, -12.98324324887284043 ) ) ;
#11092 = DIRECTION ( 'NONE',  ( 1.000000000000000000, 0.000000000000000000, -0.000000000000000000 ) ) ;
#11093 = CARTESIAN_POINT ( 'NONE',  ( 217.4999999999996305, 133.0668745871126930, -30.86484227207697018 ) ) ;
#11094 = ORIENTED_EDGE ( 'NONE', *, *, #23822, .T. ) ;
#11095 = EDGE_CURVE ( 'NONE', #24747, #9674, #26412, .T. ) ;
#11096 = DIRECTION ( 'NONE',  ( 4.540956701092242152E-16, 1.000000000000000000, 0.000000000000000000 ) ) ;
#11097 = CARTESIAN_POINT ( 'NONE',  ( 154.4185842870420799, 207.6339745962155803, -45.00000000000000000 ) ) ;
#11098 = DIRECTION ( 'NONE',  ( -0.4999999999999865108, 0.8660254037844464792, 0.000000000000000000 ) ) ;
#11099 = VERTEX_POINT ( 'NONE', #1713 ) ;
#11100 = VERTEX_POINT ( 'NONE', #24135 ) ;
#11101 = EDGE_CURVE ( 'NONE', #6472, #20401, #26132, .T. ) ;
#11102 = VECTOR ( 'NONE', #8970, 1000.000000000000114 ) ;
#11103 = CARTESIAN_POINT ( 'NONE',  ( 204.8742559748123426, 133.4291290931197977, 45.00000000000000000 ) ) ;
#11104 = CARTESIAN_POINT ( 'NONE',  ( -161.8838264660121808, 118.9755829189611802, -23.57291196158939073 ) ) ;
#11105 = ORIENTED_EDGE ( 'NONE', *, *, #19305, .T. ) ;
#11106 = AXIS2_PLACEMENT_3D ( 'NONE', #14028, #9980, #25343 ) ;
#11107 = VERTEX_POINT ( 'NONE', #12935 ) ;
#11108 = DIRECTION ( 'NONE',  ( 0.8916010070296226386, -0.4528218681377511046, 0.000000000000000000 ) ) ;
#11109 = AXIS2_PLACEMENT_3D ( 'NONE', #26071, #6816, #15175 ) ;
#11110 = CARTESIAN_POINT ( 'NONE',  ( 179.9999999999999147, 526.4263741777961059, 100.0000000000000142 ) ) ;
#11111 = VERTEX_POINT ( 'NONE', #21687 ) ;
#11112 = VERTEX_POINT ( 'NONE', #2278 ) ;
#11113 = FACE_OUTER_BOUND ( 'NONE', #340, .T. ) ;
#11114 = ADVANCED_FACE ( 'NONE', ( #137 ), #8331, .F. ) ;
#11115 = EDGE_CURVE ( 'NONE', #11368, #28220, #135, .T. ) ;
#11116 = PLANE ( 'NONE',  #9894 ) ;
#11117 = LINE ( 'NONE', #7091, #23122 ) ;
#11118 = CARTESIAN_POINT ( 'NONE',  ( 157.9999999999999432, 213.4763749774776045, 45.00000000000000000 ) ) ;
#11119 = DIRECTION ( 'NONE',  ( 0.000000000000000000, 0.000000000000000000, -1.000000000000000000 ) ) ;
#11120 = AXIS2_PLACEMENT_3D ( 'NONE', #11740, #25353, #27084 ) ;
#11121 = CARTESIAN_POINT ( 'NONE',  ( -209.9947861493998857, 60.75004723859214550, -22.65375933340435921 ) ) ;
#11122 = FACE_OUTER_BOUND ( 'NONE', #15887, .T. ) ;
#11123 = ORIENTED_EDGE ( 'NONE', *, *, #2124, .T. ) ;
#11124 = VECTOR ( 'NONE', #22437, 999.9999999999998863 ) ;
#11125 = LINE ( 'NONE', #15166, #9019 ) ;
#11126 = LINE ( 'NONE', #17727, #550 ) ;
#11128 = CARTESIAN_POINT ( 'NONE',  ( -119.0030847931093518, 214.2064521616283059, -5.000000000000002665 ) ) ;
#11127 = VECTOR ( 'NONE', #9578, 1000.000000000000114 ) ;
#11129 = DIRECTION ( 'NONE',  ( 1.000000000000000000, 0.000000000000000000, 0.000000000000000000 ) ) ;
#11130 = EDGE_LOOP ( 'NONE', ( #27309, #25975, #21133, #27806 ) ) ;
#11131 = ADVANCED_FACE ( 'NONE', ( #19535 ), #12660, .F. ) ;
#11132 = DIRECTION ( 'NONE',  ( 0.8916010070299166257, -0.4528218681371722343, 0.000000000000000000 ) ) ;
#11133 = VECTOR ( 'NONE', #23258, 999.9999999999998863 ) ;
#11134 = ORIENTED_EDGE ( 'NONE', *, *, #9025, .T. ) ;
#11135 = CARTESIAN_POINT ( 'NONE',  ( 134.9999999999998579, 244.8793018922092699, -138.9999999999999432 ) ) ;
#11136 = CARTESIAN_POINT ( 'NONE',  ( -231.1953787138147050, 65.04295872140689028, -6.836033801457077175 ) ) ;
#11137 = CARTESIAN_POINT ( 'NONE',  ( 140.6827089022704911, 249.4569214521288245, -146.9353207969096786 ) ) ;
#11138 = ORIENTED_EDGE ( 'NONE', *, *, #1320, .F. ) ;
#11139 = FILL_AREA_STYLE_COLOUR ( '', #535 ) ;
#11140 = ORIENTED_EDGE ( 'NONE', *, *, #23931, .F. ) ;
#11141 = EDGE_CURVE ( 'NONE', #17245, #15024, #26275, .T. ) ;
#11142 = CARTESIAN_POINT ( 'NONE',  ( -207.8817926630784712, 75.32300084315906474, 40.82685150828277898 ) ) ;
#11143 = ORIENTED_EDGE ( 'NONE', *, *, #21385, .F. ) ;
#11144 = CARTESIAN_POINT ( 'NONE',  ( 147.3660254037842492, 239.4185842870417673, 45.00000000000000000 ) ) ;
#11145 = ORIENTED_EDGE ( 'NONE', *, *, #2436, .F. ) ;
#11146 = EDGE_CURVE ( 'NONE', #3920, #7087, #25826, .T. ) ;
#11147 = AXIS2_PLACEMENT_3D ( 'NONE', #3542, #1396, #3403 ) ;
#11148 = EDGE_LOOP ( 'NONE', ( #14817, #7746, #8384, #11449, #14935, #22458, #5051, #23019, #24331, #16037, #2091, #618 ) ) ;
#11149 = DIRECTION ( 'NONE',  ( 1.000000000000000000, 0.000000000000000000, -0.000000000000000000 ) ) ;
#11150 = CIRCLE ( 'NONE', #13918, 58.90601976618767566 ) ;
#11151 = ORIENTED_EDGE ( 'NONE', *, *, #21347, .F. ) ;
#11152 = ORIENTED_EDGE ( 'NONE', *, *, #20508, .F. ) ;
#11153 = VECTOR ( 'NONE', #2853, 1000.000000000000000 ) ;
#11154 = CARTESIAN_POINT ( 'NONE',  ( -225.3736415174481351, 135.7651958811099178, 14.97905406095859249 ) ) ;
#11155 = CARTESIAN_POINT ( 'NONE',  ( 96.03789414443664896, 240.4739163874647261, 19.46186845664385601 ) ) ;
#11156 = AXIS2_PLACEMENT_3D ( 'NONE', #23932, #1939, #21777 ) ;
#11157 = CARTESIAN_POINT ( 'NONE',  ( 349.0018770490533484, 96.44595867864246941, -145.0000000000000000 ) ) ;
#11158 = CARTESIAN_POINT ( 'NONE',  ( 217.4999999999996305, -5.589247009368160768, 100.0000000000000142 ) ) ;
#11159 = CARTESIAN_POINT ( 'NONE',  ( 157.4999999999994884, 211.2224374737238577, 45.00000000000000000 ) ) ;
#11160 = CARTESIAN_POINT ( 'NONE',  ( 187.4999999999996305, 40.68693696324645970, -45.00000000000000000 ) ) ;
#11161 = DIRECTION ( 'NONE',  ( -1.000000000000000000, 0.000000000000000000, 0.000000000000000000 ) ) ;
#11162 = DIRECTION ( 'NONE',  ( -0.000000000000000000, 0.000000000000000000, -1.000000000000000000 ) ) ;
#11163 = DIRECTION ( 'NONE',  ( 0.000000000000000000, 0.000000000000000000, 1.000000000000000000 ) ) ;
#11164 = DIRECTION ( 'NONE',  ( 1.000000000000000000, 0.000000000000000000, -0.000000000000000000 ) ) ;
#11165 = DIRECTION ( 'NONE',  ( 1.321694076934710155E-16, -1.000000000000000000, 0.000000000000000000 ) ) ;
#11166 = CARTESIAN_POINT ( 'NONE',  ( 124.9999999999998579, 220.0000000000000284, -90.00000000000002842 ) ) ;
#11167 = VERTEX_POINT ( 'NONE', #17089 ) ;
#11168 = AXIS2_PLACEMENT_3D ( 'NONE', #18574, #7236, #13858 ) ;
#11169 = DIRECTION ( 'NONE',  ( -0.000000000000000000, -0.000000000000000000, 1.000000000000000000 ) ) ;
#11170 = VECTOR ( 'NONE', #8833, 1000.000000000000114 ) ;
#11171 = DIRECTION ( 'NONE',  ( -0.8660254037844363761, 0.5000000000000041078, -0.000000000000000000 ) ) ;
#11172 = FACE_OUTER_BOUND ( 'NONE', #25266, .T. ) ;
#11173 = CARTESIAN_POINT ( 'NONE',  ( -5.421010862427522170E-17, -1.250000000000000444, 6.997769477110050929 ) ) ;
#11174 = AXIS2_PLACEMENT_3D ( 'NONE', #2674, #9153, #683 ) ;
#11175 = ADVANCED_FACE ( 'NONE', ( #4864 ), #17559, .F. ) ;
#11176 = VERTEX_POINT ( 'NONE', #11351 ) ;
#11177 = EDGE_CURVE ( 'NONE', #28358, #268, #16094, .T. ) ;
#11178 = CARTESIAN_POINT ( 'NONE',  ( 109.4601507141043157, 253.2495769758999415, -39.14599534725524421 ) ) ;
#11179 = VERTEX_POINT ( 'NONE', #20385 ) ;
#11180 = CARTESIAN_POINT ( 'NONE',  ( -18.15202183006797299, 129.9612872840096145, -15.33564462930252681 ) ) ;
#11181 = ORIENTED_EDGE ( 'NONE', *, *, #13688, .F. ) ;
#11182 = ORIENTED_EDGE ( 'NONE', *, *, #4388, .F. ) ;
#11183 = EDGE_LOOP ( 'NONE', ( #21006, #1938, #7970, #8738 ) ) ;
#11184 = ORIENTED_EDGE ( 'NONE', *, *, #26759, .F. ) ;
#11185 = EDGE_LOOP ( 'NONE', ( #4698, #10292, #20258, #25872 ) ) ;
#11186 = EDGE_LOOP ( 'NONE', ( #9663, #9056, #6365, #6011 ) ) ;
#11187 = CIRCLE ( 'NONE', #23566, 21.49999999999999289 ) ;
#11188 = CARTESIAN_POINT ( 'NONE',  ( -141.6428522700808230, 22.24192588826928585, 80.00000000000001421 ) ) ;
#11189 = VECTOR ( 'NONE', #7084, 1000.000000000000114 ) ;
#11190 = DIRECTION ( 'NONE',  ( 1.000000000000000000, 1.541976423090495387E-16, -0.000000000000000000 ) ) ;
#11191 = VECTOR ( 'NONE', #3063, 1000.000000000000114 ) ;
#11192 = PRODUCT_DEFINITION_CONTEXT ( 'detailed design', #13339, 'design' ) ;
#11193 = LINE ( 'NONE', #15226, #19912 ) ;
#11194 = CARTESIAN_POINT ( 'NONE',  ( -217.0794644928064088, 71.41167302539513173, 24.35665452625131522 ) ) ;
#11195 = DIRECTION ( 'NONE',  ( 1.000000000000000000, -0.000000000000000000, -0.000000000000000000 ) ) ;
#11196 = CARTESIAN_POINT ( 'NONE',  ( 158.0000000000011937, 93.09837461714084839, 45.00000000000000000 ) ) ;
#11197 = ADVANCED_FACE ( 'NONE', ( #2711 ), #1506, .T. ) ;
#11198 = CYLINDRICAL_SURFACE ( 'NONE', #16353, 30.00000000000000000 ) ;
#11199 = CARTESIAN_POINT ( 'NONE',  ( -123.8208147886770121, 198.8605305197760913, -13.00000000000000000 ) ) ;
#11200 =( BOUNDED_SURFACE ( )  B_SPLINE_SURFACE ( 3, 2, ( 
 ( #3218, #24041, #21740 ),
 ( #11104, #10541, #4203 ),
 ( #8530, #23897, #17423 ),
 ( #3924, #26041, #23752 ),
 ( #21592, #19582, #17144 ),
 ( #28185, #1764, #12994 ),
 ( #28040, #17564, #6361 ),
 ( #15428, #19297, #4060 ),
 ( #4478, #17705, #8390 ),
 ( #10684, #12849, #15002 ),
 ( #19442, #4344, #25900 ),
 ( #22017, #6223, #8948 ),
 ( #21877, #2050, #10825 ),
 ( #28321, #19720, #8668 ),
 ( #2325, #15142, #26181 ),
 ( #1904, #6505, #24180 ),
 ( #15289, #13138, #12711 ),
 ( #2184, #10964, #17281 ),
 ( #43, #8802, #26322 ),
 ( #6648, #21448, #13269 ),
 ( #19861, #188, #26452 ),
 ( #14864, #23611, #15710 ),
 ( #13554, #11550, #9089 ),
 ( #20144, #22161, #15859 ),
 ( #20002, #9525, #26755 ),
 ( #7368, #2467, #24463 ) ),
 .UNSPECIFIED., .F., .F., .T. ) 
 B_SPLINE_SURFACE_WITH_KNOTS ( ( 4, 2, 2, 2, 2, 2, 2, 2, 2, 2, 2, 2, 4 ),
 ( 3, 3 ),
 ( 0.000000000000000000, 0.006475292796905446693, 0.01295058559381089339, 0.01942587839071634181, 0.02590117118762178677, 0.02913881758607450925, 0.03075764078530086876, 0.03237646398452723173, 0.03561411038297995768, 0.03885175678143268363, 0.04532704957833812859, 0.04856469597679084760, 0.05180234237524357355 ),
 ( 0.000000000000000000, 1.000000000000000000 ),
 .UNSPECIFIED. ) 
 GEOMETRIC_REPRESENTATION_ITEM ( )  RATIONAL_B_SPLINE_SURFACE ( (
 ( 1.000000000000000000, 0.8981184559478653240, 1.000000000000000000),
 ( 1.000000000000000000, 0.9063539217822286220, 1.000000000000000000),
 ( 1.000000000000000000, 0.9141583029243198766, 1.000000000000000000),
 ( 1.000000000000000000, 0.9287421046155968085, 1.000000000000000000),
 ( 1.000000000000000000, 0.9355219901798119686, 1.000000000000000000),
 ( 1.000000000000000000, 0.9478609921803489158, 1.000000000000000000),
 ( 1.000000000000000000, 0.9534203654370090320, 1.000000000000000000),
 ( 1.000000000000000000, 0.9630842474809748754, 1.000000000000000000),
 ( 1.000000000000000000, 0.9671903355926384505, 1.000000000000000000),
 ( 1.000000000000000000, 0.9720373127047674533, 1.000000000000000000),
 ( 1.000000000000000000, 0.9734336496369194736, 1.000000000000000000),
 ( 1.000000000000000000, 0.9751626172152862981, 1.000000000000000000),
 ( 1.000000000000000000, 0.9756779393314085613, 1.000000000000000000),
 ( 1.000000000000000000, 0.9765794559351392845, 1.000000000000000000),
 ( 1.000000000000000000, 0.9769664380131323211, 1.000000000000000000),
 ( 1.000000000000000000, 0.9779163903307834804, 1.000000000000000000),
 ( 1.000000000000000000, 0.9782631544368628473, 1.000000000000000000),
 ( 1.000000000000000000, 0.9783930851710932464, 1.000000000000000000),
 ( 1.000000000000000000, 0.9781763639274896338, 1.000000000000000000),
 ( 1.000000000000000000, 0.9767097374471905846, 1.000000000000000000),
 ( 1.000000000000000000, 0.9746417070090728219, 1.000000000000000000),
 ( 1.000000000000000000, 0.9700692524430989394, 1.000000000000000000),
 ( 1.000000000000000000, 0.9683033234255177257, 1.000000000000000000),
 ( 1.000000000000000000, 0.9643524362418313123, 1.000000000000000000),
 ( 1.000000000000000000, 0.9621641871898499732, 1.000000000000000000),
 ( 1.000000000000000000, 0.9597817246759324794, 1.000000000000000000) ) ) 
 REPRESENTATION_ITEM ( '' )  SURFACE ( )  );
#11201 = CARTESIAN_POINT ( 'NONE',  ( 157.9999999999997158, 261.6338751276190351, -45.00000000000000000 ) ) ;
#11202 = CARTESIAN_POINT ( 'NONE',  ( 81.45493510940914916, 110.0000000000000142, 70.00000000030220804 ) ) ;
#11203 = DIRECTION ( 'NONE',  ( -0.000000000000000000, -0.000000000000000000, -1.000000000000000000 ) ) ;
#11204 = CARTESIAN_POINT ( 'NONE',  ( -208.4180970336325913, 72.50582114360651076, 40.62062832311974603 ) ) ;
#11205 = CARTESIAN_POINT ( 'NONE',  ( 158.0000000000009948, 108.6534996696901345, 45.00000000000000000 ) ) ;
#11206 = EDGE_CURVE ( 'NONE', #20401, #5762, #3797, .T. ) ;
#11208 = ORIENTED_EDGE ( 'NONE', *, *, #26721, .F. ) ;
#11207 = ORIENTED_EDGE ( 'NONE', *, *, #8217, .T. ) ;
#11209 = CIRCLE ( 'NONE', #23588, 21.59849023212046149 ) ;
#11210 = CARTESIAN_POINT ( 'NONE',  ( -180.7514521273787125, 109.5450234118598161, 29.99853612640514200 ) ) ;
#11211 = EDGE_CURVE ( 'NONE', #3398, #16038, #13651, .T. ) ;
#11212 = EDGE_CURVE ( 'NONE', #20874, #9488, #7490, .T. ) ;
#11213 = PRODUCT_DEFINITION_SHAPE ( 'NONE', 'NONE',  #28409 ) ;
#11214 = DIRECTION ( 'NONE',  ( -0.000000000000000000, 0.000000000000000000, -1.000000000000000000 ) ) ;
#11215 = EDGE_CURVE ( 'NONE', #28035, #21416, #26161, .T. ) ;
#11216 = CARTESIAN_POINT ( 'NONE',  ( 222.4999999999996021, 186.4134324495536248, -35.02193266779035952 ) ) ;
#11217 = VERTEX_POINT ( 'NONE', #7177 ) ;
#11218 = AXIS2_PLACEMENT_3D ( 'NONE', #6770, #15276, #13259 ) ;
#11219 = ORIENTED_EDGE ( 'NONE', *, *, #11972, .F. ) ;
#11220 = ORIENTED_EDGE ( 'NONE', *, *, #5214, .F. ) ;
#11221 = CARTESIAN_POINT ( 'NONE',  ( -42.99650729631200363, 36.92584315232891612, 99.00000000000000000 ) ) ;
#11222 = CARTESIAN_POINT ( 'NONE',  ( -138.8964747619121454, 128.5890830931904816, 15.90235027539833901 ) ) ;
#11223 = ORIENTED_EDGE ( 'NONE', *, *, #27279, .F. ) ;
#11224 = EDGE_LOOP ( 'NONE', ( #19963, #14085, #25203, #10942 ) ) ;
#11225 = CARTESIAN_POINT ( 'NONE',  ( 367.4999999999996021, 44.41075299063184190, 75.00000000000004263 ) ) ;
#11226 = LINE ( 'NONE', #17679, #9593 ) ;
#11227 = ORIENTED_EDGE ( 'NONE', *, *, #13007, .F. ) ;
#11229 = CARTESIAN_POINT ( 'NONE',  ( -216.3450931143857758, 86.38378630374840839, 20.83050718481806030 ) ) ;
#11228 = ADVANCED_BREP_SHAPE_REPRESENTATION ( '', ( #8903, #10637 ), #19371 ) ;
#11230 = AXIS2_PLACEMENT_3D ( 'NONE', #16291, #7799, #20869 ) ;
#11231 = CARTESIAN_POINT ( 'NONE',  ( -211.4917091876254744, -219.2061850725015120, 107.9125863485613195 ) ) ;
#11232 = CARTESIAN_POINT ( 'NONE',  ( 157.4999999999997158, 263.8878126313725829, -45.00000000000000000 ) ) ;
#11233 = VECTOR ( 'NONE', #9589, 1000.000000000000000 ) ;
#11234 = CARTESIAN_POINT ( 'NONE',  ( 159.9606642740977520, 203.3537529630600034, -139.3072807822095456 ) ) ;
#11235 = ADVANCED_FACE ( 'NONE', ( #27131, #20096, #11647, #22111, #13799 ), #9188, .T. ) ;
#11236 = EDGE_CURVE ( 'NONE', #9426, #3254, #16235, .T. ) ;
#11237 = EDGE_LOOP ( 'NONE', ( #3980, #24149, #22528, #18771 ) ) ;
#11238 = DIRECTION ( 'NONE',  ( -0.8916010070297948342, 0.4528218681374120425, 0.000000000000000000 ) ) ;
#11239 = EDGE_CURVE ( 'NONE', #14420, #26421, #15662, .T. ) ;
#11240 = CARTESIAN_POINT ( 'NONE',  ( -223.0199379110806319, 134.9200334684691143, -15.12837422688741462 ) ) ;
#11241 = CARTESIAN_POINT ( 'NONE',  ( 157.4999999999998579, 163.5728123310915407, 45.00000000000000000 ) ) ;
#11242 = CARTESIAN_POINT ( 'NONE',  ( 157.4999999999998579, 63.25781203080982351, 45.00000000000000000 ) ) ;
#11243 = ORIENTED_EDGE ( 'NONE', *, *, #13307, .T. ) ;
#11244 = LINE ( 'NONE', #6351, #24268 ) ;
#11245 = ADVANCED_FACE ( 'NONE', ( #7029 ), #24555, .F. ) ;
#11246 = CARTESIAN_POINT ( 'NONE',  ( 109.9999999999999289, -90.00000000000001421, -100.0000000000000142 ) ) ;
#11247 = CARTESIAN_POINT ( 'NONE',  ( -142.7917509638491254, 69.37713474640312938, 82.93960292326050876 ) ) ;
#11248 = ORIENTED_EDGE ( 'NONE', *, *, #5631, .T. ) ;
#11249 =( NAMED_UNIT ( * ) SI_UNIT ( $, .STERADIAN. ) SOLID_ANGLE_UNIT ( ) );
#11250 = CIRCLE ( 'NONE', #24550, 14.94182580522077330 ) ;
#11251 = VERTEX_POINT ( 'NONE', #18935 ) ;
#11252 = AXIS2_PLACEMENT_3D ( 'NONE', #24515, #384, #6984 ) ;
#11253 = AXIS2_PLACEMENT_3D ( 'NONE', #9924, #23133, #7205 ) ;
#11254 = EDGE_CURVE ( 'NONE', #14719, #21880, #12487, .T. ) ;
#11255 = CARTESIAN_POINT ( 'NONE',  ( 157.9999999999996589, 276.1732501651540588, -45.00000000000000000 ) ) ;
#11256 = DIRECTION ( 'NONE',  ( 0.000000000000000000, -1.000000000000000000, 0.000000000000000000 ) ) ;
#11257 = ORIENTED_EDGE ( 'NONE', *, *, #15670, .T. ) ;
#11258 = AXIS2_PLACEMENT_3D ( 'NONE', #27207, #27476, #16723 ) ;
#11259 = EDGE_LOOP ( 'NONE', ( #21802, #17183, #27767, #21812 ) ) ;
#11260 = CARTESIAN_POINT ( 'NONE',  ( -125.2895325436294058, 200.2180533211638362, -13.00000000000000000 ) ) ;
#11261 = DIRECTION ( 'NONE',  ( 0.4528218681369723941, 0.8916010070300182111, -0.000000000000000000 ) ) ;
#11262 = ORIENTED_EDGE ( 'NONE', *, *, #1303, .F. ) ;
#11263 = ORIENTED_EDGE ( 'NONE', *, *, #4944, .F. ) ;
#11264 = CARTESIAN_POINT ( 'NONE',  ( -7.915935011954262635, 131.1680411804064477, 16.32730855510867585 ) ) ;
#11265 = CARTESIAN_POINT ( 'NONE',  ( 157.4999999999998579, 156.0491873085704242, 45.00000000000000000 ) ) ;
#11266 = AXIS2_PLACEMENT_3D ( 'NONE', #25357, #4633, #198 ) ;
#11267 = CARTESIAN_POINT ( 'NONE',  ( 48.74042075079900371, -13.05995637893015449, -45.00000000000000000 ) ) ;
#11268 = CARTESIAN_POINT ( 'NONE',  ( -11.50561076655487014, 131.4941894630789250, -16.18874966886875200 ) ) ;
#11269 = AXIS2_PLACEMENT_3D ( 'NONE', #8263, #17016, #25772 ) ;
#11270 = DIRECTION ( 'NONE',  ( -0.000000000000000000, -0.000000000000000000, -1.000000000000000000 ) ) ;
#11271 = CIRCLE ( 'NONE', #27305, 5.999999999999991118 ) ;
#11272 = CARTESIAN_POINT ( 'NONE',  ( -180.0000000000000284, -70.00000000000004263, 70.00000000000001421 ) ) ;
#11273 = DIRECTION ( 'NONE',  ( 0.000000000000000000, -1.000000000000000000, -1.214306433183764966E-16 ) ) ;
#11274 = EDGE_CURVE ( 'NONE', #18947, #26586, #10037, .T. ) ;
#11275 = EDGE_CURVE ( 'NONE', #7481, #16156, #16372, .T. ) ;
#11276 = VERTEX_POINT ( 'NONE', #18521 ) ;
#11277 = DIRECTION ( 'NONE',  ( -0.000000000000000000, 0.000000000000000000, -1.000000000000000000 ) ) ;
#11278 = AXIS2_PLACEMENT_3D ( 'NONE', #1443, #23423, #3732 ) ;
#11279 = LINE ( 'NONE', #17584, #8332 ) ;
#11280 = PLANE ( 'NONE',  #7307 ) ;
#11281 = CARTESIAN_POINT ( 'NONE',  ( 157.4999999999998579, 135.9861872485140850, 45.00000000000000000 ) ) ;
#11282 = VERTEX_POINT ( 'NONE', #5856 ) ;
#11283 = DIRECTION ( 'NONE',  ( -0.000000000000000000, 0.000000000000000000, -1.000000000000000000 ) ) ;
#11284 = ORIENTED_EDGE ( 'NONE', *, *, #8028, .T. ) ;
#11285 = DIRECTION ( 'NONE',  ( 0.000000000000000000, 0.000000000000000000, -1.000000000000000000 ) ) ;
#11286 = CARTESIAN_POINT ( 'NONE',  ( 157.4999999999998295, 218.7460624962465090, 45.00000000000000000 ) ) ;
#11287 = CARTESIAN_POINT ( 'NONE',  ( 139.7704065317532809, 249.6191093996066286, -141.3400049877799631 ) ) ;
#11288 = ORIENTED_EDGE ( 'NONE', *, *, #24736, .T. ) ;
#11289 = CARTESIAN_POINT ( 'NONE',  ( 157.4999999999998579, 125.9546872184859012, 45.00000000000000000 ) ) ;
#11290 = EDGE_LOOP ( 'NONE', ( #26832, #10373, #22950, #12108 ) ) ;
#11291 = EDGE_CURVE ( 'NONE', #17958, #1877, #1407, .T. ) ;
#11292 = LINE ( 'NONE', #15895, #16214 ) ;
#11293 = EDGE_LOOP ( 'NONE', ( #7960, #22860, #1170, #11328, #3289 ) ) ;
#11294 = ADVANCED_FACE ( 'NONE', ( #8018 ), #16785, .F. ) ;
#11295 = LINE ( 'NONE', #16036, #26873 ) ;
#11296 = ORIENTED_EDGE ( 'NONE', *, *, #9503, .T. ) ;
#11297 = VECTOR ( 'NONE', #15943, 1000.000000000000114 ) ;
#11298 = AXIS2_PLACEMENT_3D ( 'NONE', #332, #6785, #20432 ) ;
#11299 = ORIENTED_EDGE ( 'NONE', *, *, #24127, .T. ) ;
#11300 = CARTESIAN_POINT ( 'NONE',  ( 157.4999999999997726, 243.8248125713165280, 45.00000000000000000 ) ) ;
#11301 = ORIENTED_EDGE ( 'NONE', *, *, #12011, .F. ) ;
#11302 = ORIENTED_EDGE ( 'NONE', *, *, #14715, .F. ) ;
#11303 = AXIS2_PLACEMENT_3D ( 'NONE', #4298, #19807, #565 ) ;
#11304 = ORIENTED_EDGE ( 'NONE', *, *, #6743, .T. ) ;
#11305 = EDGE_CURVE ( 'NONE', #24279, #26566, #8159, .T. ) ;
#11306 = CARTESIAN_POINT ( 'NONE',  ( 96.65725945967196253, 241.1367295422483608, 10.34535073431436025 ) ) ;
#11307 = EDGE_CURVE ( 'NONE', #19138, #12493, #14360, .T. ) ;
#11308 = CARTESIAN_POINT ( 'NONE',  ( -26.22291647523108438, 23.54903675176048594, 45.00000000000000000 ) ) ;
#11309 = FACE_OUTER_BOUND ( 'NONE', #11183, .T. ) ;
#11310 = DIRECTION ( 'NONE',  ( -1.000000000000000000, -4.625929269271485914E-16, 0.000000000000000000 ) ) ;
#11311 = CARTESIAN_POINT ( 'NONE',  ( 157.4999999999998579, 128.4625622259929401, 45.00000000000000000 ) ) ;
#11312 = DIRECTION ( 'NONE',  ( -1.000000000000000000, 8.673617379884073683E-17, 0.000000000000000000 ) ) ;
#11313 = CARTESIAN_POINT ( 'NONE',  ( 157.9999999999997442, 251.6023750975910218, -45.00000000000000000 ) ) ;
#11314 = CARTESIAN_POINT ( 'NONE',  ( 158.0000000000006253, 146.2716247822957598, 45.00000000000000000 ) ) ;
#11315 = CARTESIAN_POINT ( 'NONE',  ( 134.9999999999998579, 220.0000000000000284, -189.9999999999999716 ) ) ;
#11316 = CARTESIAN_POINT ( 'NONE',  ( 46.79174272583949090, 194.0572550123460474, -13.00000000000000000 ) ) ;
#11317 = CARTESIAN_POINT ( 'NONE',  ( 158.0000000000016485, 50.46449948952111697, -45.00000000000000000 ) ) ;
#11318 = VECTOR ( 'NONE', #1592, 1000.000000000000227 ) ;
#11319 = ORIENTED_EDGE ( 'NONE', *, *, #5398, .T. ) ;
#11320 = CARTESIAN_POINT ( 'NONE',  ( -37.82257053376181233, 71.03850157808263077, 99.00000000000000000 ) ) ;
#11321 = CARTESIAN_POINT ( 'NONE',  ( 79.99999999999992895, 230.0000000000000284, 15.00000000000000000 ) ) ;
#11322 = DIRECTION ( 'NONE',  ( 1.000000000000000000, 2.602085213965211135E-16, 0.000000000000000000 ) ) ;
#11323 = CARTESIAN_POINT ( 'NONE',  ( 106.7205985613565105, 209.9859427875843778, -142.5205423047663942 ) ) ;
#11324 = VECTOR ( 'NONE', #14314, 1000.000000000000000 ) ;
#11325 = ORIENTED_EDGE ( 'NONE', *, *, #19437, .T. ) ;
#11326 = EDGE_CURVE ( 'NONE', #1637, #9971, #27266, .T. ) ;
#11327 = LINE ( 'NONE', #20069, #15764 ) ;
#11328 = ORIENTED_EDGE ( 'NONE', *, *, #21711, .T. ) ;
#11329 = CARTESIAN_POINT ( 'NONE',  ( -28.20602204321357576, 129.1555197674190083, -15.69110966610875657 ) ) ;
#11330 = VERTEX_POINT ( 'NONE', #25259 ) ;
#11331 = ORIENTED_EDGE ( 'NONE', *, *, #19086, .T. ) ;
#11332 = VERTEX_POINT ( 'NONE', #27820 ) ;
#11333 = VERTEX_POINT ( 'NONE', #7604 ) ;
#11334 = VERTEX_POINT ( 'NONE', #23250 ) ;
#11335 = VERTEX_POINT ( 'NONE', #18793 ) ;
#11336 = VECTOR ( 'NONE', #14032, 1000.000000000000114 ) ;
#11337 = DIRECTION ( 'NONE',  ( -0.8916010070293510781, 0.4528218681382856214, 0.000000000000000000 ) ) ;
#11338 = LINE ( 'NONE', #19412, #17083 ) ;
#11339 = DIRECTION ( 'NONE',  ( -0.000000000000000000, 0.000000000000000000, -1.000000000000000000 ) ) ;
#11340 = EDGE_CURVE ( 'NONE', #4176, #16411, #14216, .T. ) ;
#11341 = CARTESIAN_POINT ( 'NONE',  ( -20.30609983892121306, 129.6347424868099267, 15.47798682350772559 ) ) ;
#11342 = ADVANCED_FACE ( 'NONE', ( #5578 ), #5434, .F. ) ;
#11343 = CARTESIAN_POINT ( 'NONE',  ( -211.4394172367905185, 73.16162223722160718, 31.69164223700430938 ) ) ;
#11344 = LINE ( 'NONE', #4713, #15273 ) ;
#11345 = CARTESIAN_POINT ( 'NONE',  ( -160.0000000000000284, 59.99999999999994316, -45.00000000000000000 ) ) ;
#11346 = CARTESIAN_POINT ( 'NONE',  ( 158.0000000000014211, 70.52749954957745615, 45.00000000000000000 ) ) ;
#11347 = DIRECTION ( 'NONE',  ( -1.000000000000000000, 0.000000000000000000, 0.000000000000000000 ) ) ;
#11348 = EDGE_CURVE ( 'NONE', #22419, #12991, #18047, .T. ) ;
#11349 = FACE_OUTER_BOUND ( 'NONE', #10367, .T. ) ;
#11350 = CARTESIAN_POINT ( 'NONE',  ( -260.0000000000001137, -157.0000000000000284, 60.00000000000002132 ) ) ;
#11351 = CARTESIAN_POINT ( 'NONE',  ( 157.4999999999998579, 133.4783122410070462, -45.00000000000000000 ) ) ;
#11352 = DIRECTION ( 'NONE',  ( 0.8916010070299267287, -0.4528218681371523058, 0.000000000000000000 ) ) ;
#11353 = DIRECTION ( 'NONE',  ( 0.8916010070293383105, -0.4528218681383106015, 0.000000000000000000 ) ) ;
#11354 = LINE ( 'NONE', #22115, #13391 ) ;
#11355 = CARTESIAN_POINT ( 'NONE',  ( -56.65306767071049165, 63.08575069354419185, 45.00000000000000000 ) ) ;
#11357 = ORIENTED_EDGE ( 'NONE', *, *, #25525, .F. ) ;
#11356 = ORIENTED_EDGE ( 'NONE', *, *, #2998, .F. ) ;
#11358 = VECTOR ( 'NONE', #16255, 999.9999999999998863 ) ;
#11359 = CARTESIAN_POINT ( 'NONE',  ( 157.4999999999998579, 95.86018712840139244, 45.00000000000000000 ) ) ;
#11360 = DIRECTION ( 'NONE',  ( -0.000000000000000000, -0.000000000000000000, -1.000000000000000000 ) ) ;
#11361 = CARTESIAN_POINT ( 'NONE',  ( -207.4088226029311102, 90.18755115757591057, -25.68075420788710161 ) ) ;
#11362 = ORIENTED_EDGE ( 'NONE', *, *, #4736, .T. ) ;
#11363 = ITEM_DEFINED_TRANSFORMATION ( 'NONE', 'NONE', #28067,  #10637 ) ;
#11364 = VERTEX_POINT ( 'NONE', #20949 ) ;
#11365 = ORIENTED_EDGE ( 'NONE', *, *, #9592, .T. ) ;
#11366 = DIRECTION ( 'NONE',  ( 1.000000000000000000, 0.000000000000000000, 0.000000000000000000 ) ) ;
#11367 = CARTESIAN_POINT ( 'NONE',  ( -156.1148230221487552, 122.3320249483163877, 20.71187466365067564 ) ) ;
#11368 = VERTEX_POINT ( 'NONE', #22831 ) ;
#11369 = VERTEX_POINT ( 'NONE', #1266 ) ;
#11370 = CARTESIAN_POINT ( 'NONE',  ( 157.4999999999998579, 223.7618125112605298, 45.00000000000000000 ) ) ;
#11371 = TOROIDAL_SURFACE ( 'NONE', #28313, 14.95564396479129243, 3.532530335305412716 ) ;
#11372 = DIRECTION ( 'NONE',  ( 0.000000000000000000, 0.000000000000000000, -1.000000000000000000 ) ) ;
#11373 = ORIENTED_EDGE ( 'NONE', *, *, #19137, .T. ) ;
#11374 = EDGE_CURVE ( 'NONE', #17566, #25233, #14352, .T. ) ;
#11375 = CARTESIAN_POINT ( 'NONE',  ( 157.9999999999998579, 221.0000000000000284, 45.00000000000000000 ) ) ;
#11376 = CIRCLE ( 'NONE', #26037, 5.000000000000004441 ) ;
#11377 = FACE_OUTER_BOUND ( 'NONE', #6260, .T. ) ;
#11378 = EDGE_CURVE ( 'NONE', #17634, #10196, #12063, .T. ) ;
#11379 = ADVANCED_FACE ( 'NONE', ( #9899 ), #27396, .F. ) ;
#11380 = LINE ( 'NONE', #22429, #7081 ) ;
#11381 = CARTESIAN_POINT ( 'NONE',  ( 158.0000000000017337, 40.94087446699997912, 45.00000000000000000 ) ) ;
#11382 = CARTESIAN_POINT ( 'NONE',  ( -197.4451421692467079, 62.05060586452424332, -32.13681025546651426 ) ) ;
#11383 = ORIENTED_EDGE ( 'NONE', *, *, #10141, .T. ) ;
#11384 = DIRECTION ( 'NONE',  ( -0.000000000000000000, -0.000000000000000000, -1.000000000000000000 ) ) ;
#11385 = CARTESIAN_POINT ( 'NONE',  ( -236.8667578982872044, 138.8517089611673043, -5.000000000000004441 ) ) ;
#11386 = PLANE ( 'NONE',  #21662 ) ;
#11387 = LINE ( 'NONE', #324, #1118 ) ;
#11388 = VERTEX_POINT ( 'NONE', #25402 ) ;
#11389 = DIRECTION ( 'NONE',  ( -0.000000000000000000, 1.000000000000000000, -1.387778780781445429E-16 ) ) ;
#11390 = VECTOR ( 'NONE', #18237, 1000.000000000000000 ) ;
#11391 = PLANE ( 'NONE',  #2918 ) ;
#11392 = CIRCLE ( 'NONE', #377, 6.025000000000002132 ) ;
#11393 = CARTESIAN_POINT ( 'NONE',  ( 157.9999999999996874, 266.6496251426330559, 45.00000000000000000 ) ) ;
#11394 = ORIENTED_EDGE ( 'NONE', *, *, #8102, .F. ) ;
#11395 = DIRECTION ( 'NONE',  ( 1.000000000000000000, 0.000000000000000000, 0.000000000000000000 ) ) ;
#11396 = EDGE_LOOP ( 'NONE', ( #8034, #18349, #11248, #5613, #10901, #9100, #5942, #7327, #17773 ) ) ;
#11397 = DIRECTION ( 'NONE',  ( -1.321694076934710155E-16, 1.000000000000000000, 0.000000000000000000 ) ) ;
#11398 = DIRECTION ( 'NONE',  ( -0.8660254037844464792, -0.4999999999999865108, 0.000000000000000000 ) ) ;
#11399 = ORIENTED_EDGE ( 'NONE', *, *, #12095, .F. ) ;
#11400 = ORIENTED_EDGE ( 'NONE', *, *, #17090, .T. ) ;
#11401 = DIRECTION ( 'NONE',  ( -0.000000000000000000, -0.000000000000000000, 1.000000000000000000 ) ) ;
#11402 = EDGE_CURVE ( 'NONE', #14035, #194, #5718, .T. ) ;
#11403 = EDGE_CURVE ( 'NONE', #22271, #21564, #4267, .T. ) ;
#11404 = CARTESIAN_POINT ( 'NONE',  ( 367.9108539694884144, 19.41075299063184900, 80.49671038392669686 ) ) ;
#11405 = COLOUR_RGB ( '',0.7921568627450980005, 0.8196078431372548767, 0.9333333333333333481 ) ;
#11406 = EDGE_LOOP ( 'NONE', ( #16281, #10187, #23921, #14739 ) ) ;
#11407 = CARTESIAN_POINT ( 'NONE',  ( 85.37729192592163940, 80.27798593822440409, 100.0000000000000142 ) ) ;
#11408 = EDGE_LOOP ( 'NONE', ( #15711, #6010, #17746, #9532, #19559, #7924 ) ) ;
#11409 = LINE ( 'NONE', #13146, #25820 ) ;
#11410 = EDGE_CURVE ( 'NONE', #8764, #23283, #16232, .T. ) ;
#11411 = CONICAL_SURFACE ( 'NONE', #27434, 30.00000000000001421, 0.4537856055185259252 ) ;
#11412 = ADVANCED_FACE ( 'NONE', ( #8305 ), #25963, .T. ) ;
#11413 = VECTOR ( 'NONE', #12479, 1000.000000000000114 ) ;
#11414 = CARTESIAN_POINT ( 'NONE',  ( 158.0000000000011653, 93.60624962464788723, 45.00000000000000000 ) ) ;
#11415 = DIRECTION ( 'NONE',  ( 0.000000000000000000, 0.000000000000000000, 1.000000000000000000 ) ) ;
#11416 = CARTESIAN_POINT ( 'NONE',  ( -31.58116565127622621, 129.2285914189400557, -16.96974868353508370 ) ) ;
#11417 = CARTESIAN_POINT ( 'NONE',  ( 150.8670668058247202, 207.8247714198255949, 45.00000000000000000 ) ) ;
#11418 = CARTESIAN_POINT ( 'NONE',  ( 157.4999999999998579, 138.4940622560211239, -45.00000000000000000 ) ) ;
#11419 = CARTESIAN_POINT ( 'NONE',  ( 161.7276425571222092, 206.3697252471818615, -139.1927212198768871 ) ) ;
#11420 = PRODUCT_RELATED_PRODUCT_CATEGORY ( 'part', '', ( #14871 ) ) ;
#11421 = ORIENTED_EDGE ( 'NONE', *, *, #20673, .T. ) ;
#11422 = CARTESIAN_POINT ( 'NONE',  ( 367.4999999999996021, 44.41075299063184900, 1.850330238640837654E-14 ) ) ;
#11423 = CARTESIAN_POINT ( 'NONE',  ( -40.40953891503691153, 0.000000000000000000, 100.0000000000000000 ) ) ;
#11424 = CARTESIAN_POINT ( 'NONE',  ( 2.399999999999999911, 0.000000000000000000, 0.000000000000000000 ) ) ;
#11425 = CARTESIAN_POINT ( 'NONE',  ( 139.9869122110690114, 197.5248869502487139, 45.00000000000000000 ) ) ;
#11426 = ORIENTED_EDGE ( 'NONE', *, *, #28314, .T. ) ;
#11427 = CARTESIAN_POINT ( 'NONE',  ( -221.9128906662286909, 61.41899577391679088, 10.11264670733106996 ) ) ;
#11428 = VERTEX_POINT ( 'NONE', #15202 ) ;
#11429 = VECTOR ( 'NONE', #21617, 1000.000000000000000 ) ;
#11430 = DIRECTION ( 'NONE',  ( 0.9659258262890705327, 0.2588190451025121908, 0.000000000000000000 ) ) ;
#11431 = FACE_OUTER_BOUND ( 'NONE', #6930, .T. ) ;
#11432 = DIRECTION ( 'NONE',  ( 1.000000000000000000, 0.000000000000000000, 0.000000000000000000 ) ) ;
#11433 = ORIENTED_EDGE ( 'NONE', *, *, #4245, .F. ) ;
#11434 = PLANE ( 'NONE',  #19798 ) ;
#11435 = LINE ( 'NONE', #21911, #28070 ) ;
#11436 = ORIENTED_EDGE ( 'NONE', *, *, #25957, .T. ) ;
#11437 = VECTOR ( 'NONE', #17095, 1000.000000000000000 ) ;
#11438 = CARTESIAN_POINT ( 'NONE',  ( -216.5232992714898046, 71.44138874852887966, 24.86461342636829386 ) ) ;
#11439 = VERTEX_POINT ( 'NONE', #13056 ) ;
#11440 = CARTESIAN_POINT ( 'NONE',  ( -270.6366141379085093, -170.3090574957601291, -103.8655989124723504 ) ) ;
#11441 = AXIS2_PLACEMENT_3D ( 'NONE', #18125, #2596, #11532 ) ;
#11442 = VERTEX_POINT ( 'NONE', #23816 ) ;
#11443 = EDGE_CURVE ( 'NONE', #19844, #27008, #15303, .T. ) ;
#11444 = EDGE_LOOP ( 'NONE', ( #15862, #24534, #12312, #23658 ) ) ;
#11445 = LINE ( 'NONE', #27216, #16383 ) ;
#11446 = ORIENTED_EDGE ( 'NONE', *, *, #23057, .T. ) ;
#11447 = VECTOR ( 'NONE', #22891, 1000.000000000000000 ) ;
#11448 = ADVANCED_FACE ( 'NONE', ( #21801 ), #21250, .T. ) ;
#11449 = ORIENTED_EDGE ( 'NONE', *, *, #19350, .T. ) ;
#11450 = ORIENTED_EDGE ( 'NONE', *, *, #5867, .F. ) ;
#11451 = CARTESIAN_POINT ( 'NONE',  ( 105.2802062291979723, 246.7841820210157380, 28.66020632212674002 ) ) ;
#11452 = AXIS2_PLACEMENT_3D ( 'NONE', #18311, #5084, #16441 ) ;
#11453 = ADVANCED_FACE ( 'NONE', ( #28246 ), #5999, .F. ) ;
#11454 = CARTESIAN_POINT ( 'NONE',  ( 157.9999999999997726, 246.5866250825770294, 45.00000000000000000 ) ) ;
#11455 = VECTOR ( 'NONE', #11837, 999.9999999999998863 ) ;
#11456 = LINE ( 'NONE', #16330, #14 ) ;
#11457 = DIRECTION ( 'NONE',  ( 1.000000000000000000, 0.000000000000000000, 0.000000000000000000 ) ) ;
#11458 = CIRCLE ( 'NONE', #21525, 7.999999999999979572 ) ;
#11459 = CARTESIAN_POINT ( 'NONE',  ( -275.9792957272333638, -170.0000000000001137, 91.22365543927794818 ) ) ;
#11460 = DIRECTION ( 'NONE',  ( 1.000000000000000000, -1.850371707708594366E-15, 0.000000000000000000 ) ) ;
#11461 = EDGE_CURVE ( 'NONE', #23433, #13313, #25677, .T. ) ;
#11462 = CARTESIAN_POINT ( 'NONE',  ( -24.92338318254761020, 127.6681916698425567, -145.0000000000000000 ) ) ;
#11463 = LINE ( 'NONE', #24662, #23181 ) ;
#11464 = CARTESIAN_POINT ( 'NONE',  ( 157.9999999999996874, 266.1417501351260171, 45.00000000000000000 ) ) ;
#11465 = LINE ( 'NONE', #26818, #3589 ) ;
#11466 = CARTESIAN_POINT ( 'NONE',  ( 87.49999999999990052, 230.0000000000000284, 15.95262490344436657 ) ) ;
#11467 = ORIENTED_EDGE ( 'NONE', *, *, #24668, .T. ) ;
#11468 = DIRECTION ( 'NONE',  ( -1.000000000000000000, 0.000000000000000000, 0.000000000000000000 ) ) ;
#11469 = PLANE ( 'NONE',  #6415 ) ;
#11470 = CARTESIAN_POINT ( 'NONE',  ( 157.4999999999995453, 206.2066874587088989, 45.00000000000000000 ) ) ;
#11471 = CARTESIAN_POINT ( 'NONE',  ( 108.5410459154004172, 205.8592439309313136, -139.0778438077165902 ) ) ;
#11472 = ORIENTED_EDGE ( 'NONE', *, *, #10974, .F. ) ;
#11473 = EDGE_CURVE ( 'NONE', #16305, #13433, #8725, .T. ) ;
#11474 = AXIS2_PLACEMENT_3D ( 'NONE', #1023, #11541, #7640 ) ;
#11475 = CARTESIAN_POINT ( 'NONE',  ( 109.8651760759819354, 256.6126121034981225, -42.06544492442053240 ) ) ;
#11476 = VERTEX_POINT ( 'NONE', #6147 ) ;
#11477 = DIRECTION ( 'NONE',  ( -0.000000000000000000, -0.000000000000000000, -1.000000000000000000 ) ) ;
#11478 = ORIENTED_EDGE ( 'NONE', *, *, #670, .T. ) ;
#11479 = VECTOR ( 'NONE', #17631, 1000.000000000000000 ) ;
#11480 = EDGE_CURVE ( 'NONE', #14873, #7514, #22177, .T. ) ;
#11481 = VERTEX_POINT ( 'NONE', #17479 ) ;
#11482 = ORIENTED_EDGE ( 'NONE', *, *, #16464, .T. ) ;
#11483 = ORIENTED_EDGE ( 'NONE', *, *, #25881, .F. ) ;
#11484 = LINE ( 'NONE', #18640, #12287 ) ;
#11485 = CARTESIAN_POINT ( 'NONE',  ( 157.4999999999995168, 208.7145624662163925, 45.00000000000000000 ) ) ;
#11486 = DIRECTION ( 'NONE',  ( 0.000000000000000000, -1.000000000000000000, 0.000000000000000000 ) ) ;
#11487 = CARTESIAN_POINT ( 'NONE',  ( 0.000000000000000000, 0.000000000000000000, 83.00000000000001421 ) ) ;
#11488 = CARTESIAN_POINT ( 'NONE',  ( -260.0000000000001137, -152.0000000000000284, 95.00000000000000000 ) ) ;
#11489 = EDGE_CURVE ( 'NONE', #6860, #27270, #19875, .T. ) ;
#11490 = CARTESIAN_POINT ( 'NONE',  ( -219.3331038875187176, 71.26739478976685405, 22.27060053768792258 ) ) ;
#11491 = LINE ( 'NONE', #15806, #23979 ) ;
#11492 = CARTESIAN_POINT ( 'NONE',  ( 157.9999999999996305, 286.7126252026890256, 45.00000000000000000 ) ) ;
#11493 = EDGE_CURVE ( 'NONE', #749, #12783, #4405, .T. ) ;
#11494 = TOROIDAL_SURFACE ( 'NONE', #27080, 20.00000000000000355, 30.00000000000000000 ) ;
#11495 = CARTESIAN_POINT ( 'NONE',  ( 157.4999999999998579, 166.0806873385985796, -45.00000000000000000 ) ) ;
#11496 = CARTESIAN_POINT ( 'NONE',  ( -228.9609126401460344, 91.22585804526202935, -13.24624710532488514 ) ) ;
#11497 = FACE_OUTER_BOUND ( 'NONE', #12438, .T. ) ;
#11498 = CARTESIAN_POINT ( 'NONE',  ( -110.3221550338875687, 80.49308115506423178, 248.5795775865965993 ) ) ;
#11499 = DIRECTION ( 'NONE',  ( 0.000000000000000000, 0.000000000000000000, 1.000000000000000000 ) ) ;
#11500 = AXIS2_PLACEMENT_3D ( 'NONE', #14567, #23322, #3630 ) ;
#11501 =( REPRESENTATION_RELATIONSHIP ('NONE','NONE', #11963, #14145 ) REPRESENTATION_RELATIONSHIP_WITH_TRANSFORMATION ( #24424 )SHAPE_REPRESENTATION_RELATIONSHIP( ) );
#11502 = CARTESIAN_POINT ( 'NONE',  ( -143.6428522700808230, 20.24192588826928585, 83.00000000000001421 ) ) ;
#11503 = DIRECTION ( 'NONE',  ( 2.602085213965211135E-16, -1.000000000000000000, 0.000000000000000000 ) ) ;
#11504 = LINE ( 'NONE', #20244, #1887 ) ;
#11505 = CYLINDRICAL_SURFACE ( 'NONE', #8399, 5.999999999999991118 ) ;
#11507 = ORIENTED_EDGE ( 'NONE', *, *, #25656, .F. ) ;
#11506 = ORIENTED_EDGE ( 'NONE', *, *, #17685, .T. ) ;
#11508 = EDGE_CURVE ( 'NONE', #27514, #13811, #2244, .T. ) ;
#11509 = DIRECTION ( 'NONE',  ( 0.4528218681371711241, -0.8916010070299172918, 0.000000000000000000 ) ) ;
#11510 = DIRECTION ( 'NONE',  ( 0.000000000000000000, 0.000000000000000000, 1.000000000000000000 ) ) ;
#11511 = ORIENTED_EDGE ( 'NONE', *, *, #6623, .F. ) ;
#11512 = EDGE_LOOP ( 'NONE', ( #15010, #24645, #8406, #25710 ) ) ;
#11513 = EDGE_CURVE ( 'NONE', #22677, #6513, #16921, .T. ) ;
#11515 = ADVANCED_FACE ( 'NONE', ( #12630, #10456 ), #19217, .T. ) ;
#11514 = ORIENTED_EDGE ( 'NONE', *, *, #3474, .T. ) ;
#11516 = DIRECTION ( 'NONE',  ( -0.8916010070293283185, -0.4528218681383305855, 0.000000000000000000 ) ) ;
#11517 = AXIS2_PLACEMENT_3D ( 'NONE', #15194, #4677, #11310 ) ;
#11518 = LINE ( 'NONE', #7337, #16362 ) ;
#11519 = ORIENTED_EDGE ( 'NONE', *, *, #27281, .T. ) ;
#11520 = EDGE_CURVE ( 'NONE', #1215, #9638, #14920, .T. ) ;
#11521 = ORIENTED_EDGE ( 'NONE', *, *, #12776, .T. ) ;
#11522 = DIRECTION ( 'NONE',  ( 1.000000000000000000, -0.000000000000000000, -0.000000000000000000 ) ) ;
#11523 = FACE_OUTER_BOUND ( 'NONE', #16690, .T. ) ;
#11524 = AXIS2_PLACEMENT_3D ( 'NONE', #11320, #23961, #8592 ) ;
#11525 = CARTESIAN_POINT ( 'NONE',  ( 20.92655468430566756, 155.3461090732848220, -13.00000000000000000 ) ) ;
#11526 = VERTEX_POINT ( 'NONE', #8449 ) ;
#11527 = CARTESIAN_POINT ( 'NONE',  ( -205.8198834057387785, 91.09083988932387399, 26.98970021333139613 ) ) ;
#11528 = CARTESIAN_POINT ( 'NONE',  ( 157.4999999999998295, 231.2854375337815327, -45.00000000000000000 ) ) ;
#11529 = AXIS2_PLACEMENT_3D ( 'NONE', #5316, #11522, #20260 ) ;
#11530 = CARTESIAN_POINT ( 'NONE',  ( 157.9999999999998295, 228.5236250225210313, 45.00000000000000000 ) ) ;
#11531 = EDGE_CURVE ( 'NONE', #27897, #27519, #12909, .T. ) ;
#11532 = DIRECTION ( 'NONE',  ( -1.000000000000000000, -1.850371707708595056E-16, 0.000000000000000000 ) ) ;
#11533 = CARTESIAN_POINT ( 'NONE',  ( -216.3679220181670360, 71.52319660855025063, -25.09443459582657709 ) ) ;
#11534 = ORIENTED_EDGE ( 'NONE', *, *, #1441, .F. ) ;
#11535 = CIRCLE ( 'NONE', #27549, 1.999999999999993339 ) ;
#11536 = CARTESIAN_POINT ( 'NONE',  ( 158.0000000000014211, 73.03537455708450921, 45.00000000000000000 ) ) ;
#11537 = CARTESIAN_POINT ( 'NONE',  ( 137.6105238444012286, 200.1711027725236534, 45.00000000000000000 ) ) ;
#11538 = CARTESIAN_POINT ( 'NONE',  ( -210.0000000000000568, -152.0000000000000284, 105.0000000000000284 ) ) ;
#11539 = DIRECTION ( 'NONE',  ( -1.000000000000000000, 0.000000000000000000, -0.000000000000000000 ) ) ;
#11540 = ORIENTED_EDGE ( 'NONE', *, *, #17869, .F. ) ;
#11541 = DIRECTION ( 'NONE',  ( 1.000000000000000000, 0.000000000000000000, -0.000000000000000000 ) ) ;
#11542 = AXIS2_PLACEMENT_3D ( 'NONE', #21838, #23705, #2143 ) ;
#11543 = CARTESIAN_POINT ( 'NONE',  ( -238.3574390336322040, 69.78222348740347059, 5.410870504207573539 ) ) ;
#11544 = DIRECTION ( 'NONE',  ( 0.000000000000000000, 0.000000000000000000, 1.000000000000000000 ) ) ;
#11545 = VERTEX_POINT ( 'NONE', #9447 ) ;
#11546 = ORIENTED_EDGE ( 'NONE', *, *, #1096, .F. ) ;
#11547 = EDGE_CURVE ( 'NONE', #17151, #24242, #2526, .T. ) ;
#11548 = EDGE_CURVE ( 'NONE', #26033, #15470, #15628, .T. ) ;
#11549 = CARTESIAN_POINT ( 'NONE',  ( 100.5794065449870942, 118.1137289701970872, 81.24999999968734699 ) ) ;
#11550 = CARTESIAN_POINT ( 'NONE',  ( -200.0701886854841689, 95.67681652162154649, -30.66283971992370638 ) ) ;
#11551 = VERTEX_POINT ( 'NONE', #4970 ) ;
#11552 = ORIENTED_EDGE ( 'NONE', *, *, #16340, .F. ) ;
#11553 = CARTESIAN_POINT ( 'NONE',  ( -189.8086322075389774, 92.49158130768422836, -13.00000000000000000 ) ) ;
#11554 = AXIS2_PLACEMENT_3D ( 'NONE', #8016, #1551, #23672 ) ;
#11555 = CARTESIAN_POINT ( 'NONE',  ( 158.0000000000005684, 153.2873747973098659, -45.00000000000000000 ) ) ;
#11556 = ORIENTED_EDGE ( 'NONE', *, *, #2518, .T. ) ;
#11557 = DIRECTION ( 'NONE',  ( -0.8916010070296124246, -0.4528218681377710886, 0.000000000000000000 ) ) ;
#11558 = VERTEX_POINT ( 'NONE', #24233 ) ;
#11559 = CIRCLE ( 'NONE', #25760, 6.000000000000005329 ) ;
#11560 = CYLINDRICAL_SURFACE ( 'NONE', #2434, 5.000000000000004441 ) ;
#11561 = CIRCLE ( 'NONE', #11088, 10.00000000000000888 ) ;
#11562 = CARTESIAN_POINT ( 'NONE',  ( 158.0000000000001137, 195.9212499249295831, 45.00000000000000000 ) ) ;
#11563 = LINE ( 'NONE', #21889, #17616 ) ;
#11564 = DIRECTION ( 'NONE',  ( 1.000000000000000000, -0.000000000000000000, -0.000000000000000000 ) ) ;
#11565 = CARTESIAN_POINT ( 'NONE',  ( 48.45469728424487244, 192.9461374953035033, -13.00000000000000000 ) ) ;
#11566 = LINE ( 'NONE', #25182, #11447 ) ;
#11567 = ORIENTED_EDGE ( 'NONE', *, *, #5559, .F. ) ;
#11568 = EDGE_CURVE ( 'NONE', #1420, #11388, #534, .T. ) ;
#11569 = DIRECTION ( 'NONE',  ( -0.8916010070295616874, -0.4528218681378710642, 0.000000000000000000 ) ) ;
#11570 = CARTESIAN_POINT ( 'NONE',  ( 158.0000000000003979, 170.8424998498591663, -45.00000000000000000 ) ) ;
#11571 = LINE ( 'NONE', #20312, #13273 ) ;
#11572 = LINE ( 'NONE', #211, #26312 ) ;
#11573 = ORIENTED_EDGE ( 'NONE', *, *, #6331, .T. ) ;
#11574 = CARTESIAN_POINT ( 'NONE',  ( -244.5479615644635487, 75.99513337129094737, 5.000000000000002665 ) ) ;
#11575 = ORIENTED_EDGE ( 'NONE', *, *, #10351, .F. ) ;
#11576 = AXIS2_PLACEMENT_3D ( 'NONE', #4930, #5225, #5080 ) ;
#11577 = CARTESIAN_POINT ( 'NONE',  ( 367.9108539694884144, 19.41075299063184900, 95.49671038392668265 ) ) ;
#11578 = CARTESIAN_POINT ( 'NONE',  ( -225.0350560533458690, 62.39407306348317661, -8.837833373942165949 ) ) ;
#11579 = CARTESIAN_POINT ( 'NONE',  ( 140.9608704376672108, 249.4019415319914117, -144.2111520032348722 ) ) ;
#11580 = EDGE_LOOP ( 'NONE', ( #25097, #18556, #3845, #27592, #20783 ) ) ;
#11581 =( NAMED_UNIT ( * ) SI_UNIT ( $, .STERADIAN. ) SOLID_ANGLE_UNIT ( ) );
#11582 =( LENGTH_UNIT ( ) NAMED_UNIT ( * ) SI_UNIT ( .MILLI., .METRE. ) );
#11583 = ADVANCED_FACE ( 'NONE', ( #24373 ), #2905, .F. ) ;
#11584 = AXIS2_PLACEMENT_3D ( 'NONE', #28039, #14863, #1903 ) ;
#11585 = VERTEX_POINT ( 'NONE', #13617 ) ;
#11586 = AXIS2_PLACEMENT_3D ( 'NONE', #22303, #7073, #11395 ) ;
#11587 = EDGE_CURVE ( 'NONE', #11476, #21473, #20059, .T. ) ;
#11588 = VECTOR ( 'NONE', #24785, 1000.000000000000000 ) ;
#11589 = CARTESIAN_POINT ( 'NONE',  ( -92.70792463290142393, 134.7647503918266239, 15.46030987956200420 ) ) ;
#11590 = ORIENTED_EDGE ( 'NONE', *, *, #10242, .F. ) ;
#11591 = EDGE_CURVE ( 'NONE', #26681, #4224, #5118, .T. ) ;
#11592 = PLANE ( 'NONE',  #7622 ) ;
#11593 = ORIENTED_EDGE ( 'NONE', *, *, #7675, .T. ) ;
#11594 = ORIENTED_EDGE ( 'NONE', *, *, #17975, .T. ) ;
#11595 = DIRECTION ( 'NONE',  ( 0.000000000000000000, -2.498359269027536814E-16, 1.000000000000000000 ) ) ;
#11596 = ORIENTED_EDGE ( 'NONE', *, *, #3390, .F. ) ;
#11597 = ORIENTED_EDGE ( 'NONE', *, *, #4290, .F. ) ;
#11598 = ORIENTED_EDGE ( 'NONE', *, *, #16469, .T. ) ;
#11599 = CARTESIAN_POINT ( 'NONE',  ( 92.84236432024050600, 239.7913859916842227, 17.77233924293420841 ) ) ;
#11600 = AXIS2_PLACEMENT_3D ( 'NONE', #16819, #3875, #21261 ) ;
#11601 = CARTESIAN_POINT ( 'NONE',  ( 6.071532165918828775E-15, -70.00000000000002842, 100.0000000000000142 ) ) ;
#11602 = CARTESIAN_POINT ( 'NONE',  ( 95.82124051657368113, -20.23615780638419182, 45.00000000000000000 ) ) ;
#11603 = VECTOR ( 'NONE', #5171, 1000.000000000000000 ) ;
#11604 = AXIS2_PLACEMENT_3D ( 'NONE', #2394, #2685, #13478 ) ;
#11605 = DIRECTION ( 'NONE',  ( 0.000000000000000000, -1.000000000000000000, 0.000000000000000000 ) ) ;
#11606 = DIRECTION ( 'NONE',  ( 0.8916010070293409751, 0.4528218681383056610, 0.000000000000000000 ) ) ;
#11607 = CYLINDRICAL_SURFACE ( 'NONE', #4229, 30.00000000000000000 ) ;
#11608 = DIRECTION ( 'NONE',  ( 0.000000000000000000, 0.000000000000000000, -1.000000000000000000 ) ) ;
#11609 = CARTESIAN_POINT ( 'NONE',  ( 79.99999999999990052, 230.0000000000000284, -45.00000000000000000 ) ) ;
#11610 = DIRECTION ( 'NONE',  ( 1.224646799147353207E-16, 1.000000000000000000, -0.000000000000000000 ) ) ;
#11611 = DIRECTION ( 'NONE',  ( 0.8916010070293710621, -0.4528218681382463195, 0.000000000000000000 ) ) ;
#11612 = DIRECTION ( 'NONE',  ( 0.000000000000000000, 0.000000000000000000, 1.000000000000000000 ) ) ;
#11613 = ORIENTED_EDGE ( 'NONE', *, *, #24459, .T. ) ;
#11614 = DIRECTION ( 'NONE',  ( 0.000000000000000000, 0.000000000000000000, -1.000000000000000000 ) ) ;
#11615 = EDGE_CURVE ( 'NONE', #962, #11738, #24522, .T. ) ;
#11616 = DIRECTION ( 'NONE',  ( -0.000000000000000000, -0.000000000000000000, -1.000000000000000000 ) ) ;
#11617 = CARTESIAN_POINT ( 'NONE',  ( -15.28840184913744515, 9.956927649352207865, 45.00000000000000000 ) ) ;
#11618 = VECTOR ( 'NONE', #2988, 1000.000000000000000 ) ;
#11619 = CARTESIAN_POINT ( 'NONE',  ( 158.0000000000010516, 105.6377496546760568, -45.00000000000000000 ) ) ;
#11620 = ORIENTED_EDGE ( 'NONE', *, *, #13063, .T. ) ;
#11621 = VECTOR ( 'NONE', #12214, 1000.000000000000114 ) ;
#11622 = CARTESIAN_POINT ( 'NONE',  ( 109.2808348379079462, 254.3902513977343176, -38.18180188067670855 ) ) ;
#11623 = ORIENTED_EDGE ( 'NONE', *, *, #16944, .T. ) ;
#11624 = EDGE_CURVE ( 'NONE', #16770, #689, #22513, .T. ) ;
#11625 = CONICAL_SURFACE ( 'NONE', #5627, 6.025000000000002132, 0.7853981633974482790 ) ;
#11626 = ORIENTED_EDGE ( 'NONE', *, *, #5112, .T. ) ;
#11627 = VECTOR ( 'NONE', #10012, 1000.000000000000114 ) ;
#11628 = ADVANCED_FACE ( 'NONE', ( #22658 ), #2817, .F. ) ;
#11629 = ORIENTED_EDGE ( 'NONE', *, *, #11746, .F. ) ;
#11630 = ORIENTED_EDGE ( 'NONE', *, *, #24053, .T. ) ;
#11631 = ORIENTED_EDGE ( 'NONE', *, *, #16555, .F. ) ;
#11632 = CARTESIAN_POINT ( 'NONE',  ( 109.9999999999999432, 2.035408878479452500E-14, 45.00000000000000000 ) ) ;
#11633 = DIRECTION ( 'NONE',  ( 0.4528218681382856770, 0.8916010070293511891, -0.000000000000000000 ) ) ;
#11634 = CARTESIAN_POINT ( 'NONE',  ( 157.9999999999996589, 281.1890001801680796, 45.00000000000000000 ) ) ;
#11635 = DIRECTION ( 'NONE',  ( -0.8916010070295715684, 0.4528218681378515797, 0.000000000000000000 ) ) ;
#11636 = FACE_OUTER_BOUND ( 'NONE', #13953, .T. ) ;
#11637 = VECTOR ( 'NONE', #13278, 1000.000000000000114 ) ;
#11638 = LINE ( 'NONE', #1259, #21265 ) ;
#11639 = CARTESIAN_POINT ( 'NONE',  ( 111.3836151241014960, 219.3130464734738325, 45.00000000000000000 ) ) ;
#11640 = CARTESIAN_POINT ( 'NONE',  ( -67.45133076571056563, 135.5141271316668394, -13.65948042911834470 ) ) ;
#11641 = AXIS2_PLACEMENT_3D ( 'NONE', #28347, #15316, #4372 ) ;
#11642 = CARTESIAN_POINT ( 'NONE',  ( 134.9999999999998579, 220.0000000000000284, -105.0000000000000284 ) ) ;
#11643 = CARTESIAN_POINT ( 'NONE',  ( -203.1779787704217313, 93.05164332230201296, -28.77272332722132475 ) ) ;
#11644 = VECTOR ( 'NONE', #8865, 1000.000000000000227 ) ;
#11645 = CARTESIAN_POINT ( 'NONE',  ( -217.0264852877946566, -91.18033988749901653, 19.68410787789781580 ) ) ;
#11646 = FACE_OUTER_BOUND ( 'NONE', #21999, .T. ) ;
#11647 = FACE_BOUND ( 'NONE', #5902, .T. ) ;
#11648 = EDGE_CURVE ( 'NONE', #11251, #8811, #20786, .T. ) ;
#11649 = CARTESIAN_POINT ( 'NONE',  ( -8.429728459452139333, 132.5274614703484133, 14.39831780793436522 ) ) ;
#11650 = DIRECTION ( 'NONE',  ( -0.000000000000000000, -0.000000000000000000, -1.000000000000000000 ) ) ;
#11651 = DIRECTION ( 'NONE',  ( -0.000000000000000000, -0.000000000000000000, -1.000000000000000000 ) ) ;
#11652 = DIRECTION ( 'NONE',  ( -0.000000000000000000, 1.000000000000000000, -1.387778780781445429E-16 ) ) ;
#11654 = ORIENTED_EDGE ( 'NONE', *, *, #13325, .T. ) ;
#11653 = VERTEX_POINT ( 'NONE', #11466 ) ;
#11655 = CARTESIAN_POINT ( 'NONE',  ( -203.2481855153402250, 92.57460631283319685, -29.78692811926998729 ) ) ;
#11656 = DIRECTION ( 'NONE',  ( 1.000000000000000000, 0.000000000000000000, -0.000000000000000000 ) ) ;
#11657 = ORIENTED_EDGE ( 'NONE', *, *, #16813, .T. ) ;
#11658 = AXIS2_PLACEMENT_3D ( 'NONE', #8326, #1845, #10624 ) ;
#11659 = ORIENTED_EDGE ( 'NONE', *, *, #11868, .T. ) ;
#11660 = EDGE_CURVE ( 'NONE', #1387, #27519, #20351, .T. ) ;
#11661 = AXIS2_PLACEMENT_3D ( 'NONE', #7731, #20657, #22958 ) ;
#11662 = FACE_BOUND ( 'NONE', #28112, .T. ) ;
#11663 = EDGE_CURVE ( 'NONE', #26863, #2835, #14377, .T. ) ;
#11664 = CARTESIAN_POINT ( 'NONE',  ( -137.6856056883401322, 128.9562719326160334, 15.73927209086268064 ) ) ;
#11665 = EDGE_LOOP ( 'NONE', ( #26967, #16905, #25977, #8842 ) ) ;
#11666 = VECTOR ( 'NONE', #17444, 1000.000000000000114 ) ;
#11667 = ORIENTED_EDGE ( 'NONE', *, *, #14879, .T. ) ;
#11668 = CYLINDRICAL_SURFACE ( 'NONE', #11529, 5.999999999999991118 ) ;
#11669 = CARTESIAN_POINT ( 'NONE',  ( 158.0000000000005400, 155.7952498048169048, 45.00000000000000000 ) ) ;
#11670 = DIRECTION ( 'NONE',  ( 0.000000000000000000, 0.000000000000000000, -1.000000000000000000 ) ) ;
#11671 = VERTEX_POINT ( 'NONE', #4829 ) ;
#11672 = CARTESIAN_POINT ( 'NONE',  ( -203.8967259421660572, 92.43987101052316291, 29.06044879621326160 ) ) ;
#11673 = DIRECTION ( 'NONE',  ( 0.000000000000000000, -1.000000000000000000, 0.000000000000000000 ) ) ;
#11674 = EDGE_CURVE ( 'NONE', #23784, #13456, #2385, .T. ) ;
#11675 = EDGE_CURVE ( 'NONE', #25368, #800, #391, .T. ) ;
#11676 = FACE_OUTER_BOUND ( 'NONE', #11186, .T. ) ;
#11677 = DIRECTION ( 'NONE',  ( 0.4528218681375119625, 0.8916010070297440970, -0.000000000000000000 ) ) ;
#11678 = CARTESIAN_POINT ( 'NONE',  ( -195.0250397031994112, 62.90385929084195737, -38.63509848415888115 ) ) ;
#11679 = FACE_OUTER_BOUND ( 'NONE', #9464, .T. ) ;
#11680 = EDGE_CURVE ( 'NONE', #11684, #21857, #23553, .T. ) ;
#11681 = CARTESIAN_POINT ( 'NONE',  ( 158.0000000000003979, 170.8424998498591663, 45.00000000000000000 ) ) ;
#11682 = AXIS2_PLACEMENT_3D ( 'NONE', #18685, #16266, #16126 ) ;
#11683 = CARTESIAN_POINT ( 'NONE',  ( -160.0000000000000284, 59.99999999999994316, 15.00000000000000000 ) ) ;
#11684 = VERTEX_POINT ( 'NONE', #26661 ) ;
#11685 = DIRECTION ( 'NONE',  ( 0.000000000000000000, 0.000000000000000000, -1.000000000000000000 ) ) ;
#11686 = CARTESIAN_POINT ( 'NONE',  ( -239.3181950532627980, 70.57797675262781922, 14.71337737012095559 ) ) ;
#11687 = PLANE ( 'NONE',  #12658 ) ;
#11688 = ORIENTED_EDGE ( 'NONE', *, *, #18445, .F. ) ;
#11689 = ORIENTED_EDGE ( 'NONE', *, *, #17253, .T. ) ;
#11690 = CARTESIAN_POINT ( 'NONE',  ( -119.0030847931093518, 214.2064521616283059, 5.000000000000002665 ) ) ;
#11691 = DIRECTION ( 'NONE',  ( 0.000000000000000000, 0.000000000000000000, 1.000000000000000000 ) ) ;
#11692 = VERTEX_POINT ( 'NONE', #7139 ) ;
#11693 = VECTOR ( 'NONE', #11841, 1000.000000000000000 ) ;
#11694 = VERTEX_POINT ( 'NONE', #18207 ) ;
#11695 = LINE ( 'NONE', #22452, #26014 ) ;
#11696 = CARTESIAN_POINT ( 'NONE',  ( 134.9999999999998579, 220.0000000000000284, 99.00000000000001421 ) ) ;
#11697 = CARTESIAN_POINT ( 'NONE',  ( -215.4886702565631538, 139.8420026707765942, 14.99999999999998579 ) ) ;
#11698 = VERTEX_POINT ( 'NONE', #15918 ) ;
#11699 = CARTESIAN_POINT ( 'NONE',  ( -260.0000000000001137, -157.0000000000000284, -59.99999999999986500 ) ) ;
#11700 = EDGE_LOOP ( 'NONE', ( #8191, #10146, #471, #19586 ) ) ;
#11701 = AXIS2_PLACEMENT_3D ( 'NONE', #15782, #11322, #9016 ) ;
#11702 = LINE ( 'NONE', #20580, #13004 ) ;
#11703 = CARTESIAN_POINT ( 'NONE',  ( 282.4999999999996589, 19.41075299063184900, 95.49671038392668265 ) ) ;
#11704 = FACE_OUTER_BOUND ( 'NONE', #12856, .T. ) ;
#11705 = CARTESIAN_POINT ( 'NONE',  ( -24.85022236748708124, 129.2502597746190816, -15.64835883620313517 ) ) ;
#11706 = FACE_OUTER_BOUND ( 'NONE', #12045, .T. ) ;
#11707 = ADVANCED_FACE ( 'NONE', ( #4542 ), #6704, .F. ) ;
#11708 = DIRECTION ( 'NONE',  ( 1.000000000000000000, 2.696301922142074142E-31, -2.220446049250266932E-15 ) ) ;
#11709 = DIRECTION ( 'NONE',  ( 0.000000000000000000, -1.000000000000000000, 0.000000000000000000 ) ) ;
#11710 = ORIENTED_EDGE ( 'NONE', *, *, #27121, .F. ) ;
#11711 = FACE_BOUND ( 'NONE', #1472, .T. ) ;
#11712 = AXIS2_PLACEMENT_3D ( 'NONE', #13899, #22786, #7564 ) ;
#11713 = EDGE_CURVE ( 'NONE', #7659, #25070, #24457, .T. ) ;
#11714 = LINE ( 'NONE', #11570, #24386 ) ;
#11715 = CARTESIAN_POINT ( 'NONE',  ( -277.2150368962633706, -237.2150368962634559, 95.00000000000004263 ) ) ;
#11716 = CARTESIAN_POINT ( 'NONE',  ( -13.93137870332982331, 8.043285244550061108, 45.00000000000000000 ) ) ;
#11717 = ORIENTED_EDGE ( 'NONE', *, *, #22068, .T. ) ;
#11718 = CIRCLE ( 'NONE', #24533, 5.000000000000004441 ) ;
#11719 = LINE ( 'NONE', #7396, #27919 ) ;
#11720 = EDGE_LOOP ( 'NONE', ( #12532, #22676, #8932, #20605 ) ) ;
#11721 = LINE ( 'NONE', #7254, #18043 ) ;
#11722 = PLANE ( 'NONE',  #17877 ) ;
#11723 = LINE ( 'NONE', #18030, #18124 ) ;
#11724 = EDGE_LOOP ( 'NONE', ( #26453, #1731, #19590, #26644, #24315, #27182, #5727, #6893 ) ) ;
#11725 = LINE ( 'NONE', #27209, #4182 ) ;
#11726 = SURFACE_SIDE_STYLE ('',( #22484 ) ) ;
#11727 = CIRCLE ( 'NONE', #7589, 14.94182580522077330 ) ;
#11728 = EDGE_LOOP ( 'NONE', ( #13743, #10193, #16324, #22801 ) ) ;
#11729 = LINE ( 'NONE', #7261, #12497 ) ;
#11730 = LINE ( 'NONE', #16176, #13597 ) ;
#11731 = VERTEX_POINT ( 'NONE', #16612 ) ;
#11732 = ORIENTED_EDGE ( 'NONE', *, *, #13007, .T. ) ;
#11733 = CARTESIAN_POINT ( 'NONE',  ( -17.24491960465746132, 80.97823757117562593, 95.00000000000000000 ) ) ;
#11734 = ORIENTED_EDGE ( 'NONE', *, *, #22462, .F. ) ;
#11735 = EDGE_CURVE ( 'NONE', #14223, #9726, #16753, .T. ) ;
#11736 = CIRCLE ( 'NONE', #10810, 50.00000000000000000 ) ;
#11737 = ORIENTED_EDGE ( 'NONE', *, *, #8314, .T. ) ;
#11738 = VERTEX_POINT ( 'NONE', #10001 ) ;
#11739 = VECTOR ( 'NONE', #4119, 1000.000000000000000 ) ;
#11740 = CARTESIAN_POINT ( 'NONE',  ( -160.0000000000000284, 59.99999999999994316, 80.00000000000001421 ) ) ;
#11741 = PLANE ( 'NONE',  #20427 ) ;
#11742 = ADVANCED_FACE ( 'NONE', ( #7427 ), #23214, .T. ) ;
#11743 = CARTESIAN_POINT ( 'NONE',  ( -210.7172313291012529, 103.7585653882801182, -5.000000000000004441 ) ) ;
#11744 = AXIS2_PLACEMENT_3D ( 'NONE', #17294, #10555, #15157 ) ;
#11745 = ADVANCED_FACE ( 'NONE', ( #9724 ), #12171, .F. ) ;
#11746 = EDGE_CURVE ( 'NONE', #23197, #1515, #2442, .T. ) ;
#11747 = CARTESIAN_POINT ( 'NONE',  ( 157.4999999999998010, 238.8090625563025071, 45.00000000000000000 ) ) ;
#11748 = FACE_OUTER_BOUND ( 'NONE', #27604, .T. ) ;
#11749 = DIRECTION ( 'NONE',  ( -1.000000000000000000, 0.000000000000000000, -0.000000000000000000 ) ) ;
#11750 = EDGE_CURVE ( 'NONE', #27752, #5346, #18484, .T. ) ;
#11751 = DIRECTION ( 'NONE',  ( 1.000000000000000000, 0.000000000000000000, 0.000000000000000000 ) ) ;
#11752 = LINE ( 'NONE', #22655, #26852 ) ;
#11753 = CARTESIAN_POINT ( 'NONE',  ( -261.1919288306253293, -171.9377729149742038, 110.0000000000000142 ) ) ;
#11754 = DIRECTION ( 'NONE',  ( 0.000000000000000000, 1.272130549049657961E-16, -1.000000000000000000 ) ) ;
#11755 = CARTESIAN_POINT ( 'NONE',  ( 157.9999999999998295, 224.0157500150140208, 45.00000000000000000 ) ) ;
#11756 = ORIENTED_EDGE ( 'NONE', *, *, #17413, .T. ) ;
#11757 = CARTESIAN_POINT ( 'NONE',  ( 0.3651377029009472142, -1.250000000000000444, 7.402212548643258394 ) ) ;
#11758 = CARTESIAN_POINT ( 'NONE',  ( 232.4999999999996305, 83.06687458711267880, -36.86484227207694175 ) ) ;
#11759 = AXIS2_PLACEMENT_3D ( 'NONE', #26613, #25043, #11980 ) ;
#11760 = DIRECTION ( 'NONE',  ( 1.000000000000000000, -0.000000000000000000, -0.000000000000000000 ) ) ;
#11761 = ORIENTED_EDGE ( 'NONE', *, *, #7697, .F. ) ;
#11762 = AXIS2_PLACEMENT_3D ( 'NONE', #27518, #1666, #10436 ) ;
#11763 = LINE ( 'NONE', #18631, #8402 ) ;
#11764 = EDGE_LOOP ( 'NONE', ( #17730, #14685, #7512, #3877 ) ) ;
#11765 = PLANE ( 'NONE',  #24229 ) ;
#11766 = ORIENTED_EDGE ( 'NONE', *, *, #10775, .F. ) ;
#11767 = VERTEX_POINT ( 'NONE', #3381 ) ;
#11768 = ORIENTED_EDGE ( 'NONE', *, *, #24362, .F. ) ;
#11769 = EDGE_LOOP ( 'NONE', ( #8942, #12646, #14166, #6792 ) ) ;
#11770 = CARTESIAN_POINT ( 'NONE',  ( -158.6438865070083750, 121.2377615292502782, 20.46887661539795644 ) ) ;
#11771 = DIRECTION ( 'NONE',  ( -0.000000000000000000, -0.000000000000000000, -1.000000000000000000 ) ) ;
#11772 = LINE ( 'NONE', #27525, #20304 ) ;
#11773 = EDGE_CURVE ( 'NONE', #4407, #2835, #27507, .T. ) ;
#11774 = EDGE_CURVE ( 'NONE', #12605, #2227, #819, .T. ) ;
#11775 = CARTESIAN_POINT ( 'NONE',  ( -97.72577305530073488, 134.4685796935967801, -15.51422881674326604 ) ) ;
#11776 = UNCERTAINTY_MEASURE_WITH_UNIT (LENGTH_MEASURE( 1.000000000000000082E-05 ), #25645, 'distance_accuracy_value', 'NONE');
#11777 = VECTOR ( 'NONE', #8431, 1000.000000000000000 ) ;
#11778 = CARTESIAN_POINT ( 'NONE',  ( -40.35425475217338942, 130.4208791593096350, 15.14570953137466880 ) ) ;
#11779 = CARTESIAN_POINT ( 'NONE',  ( 158.0000000000013927, 75.54324956459154805, 45.00000000000000000 ) ) ;
#11780 = CARTESIAN_POINT ( 'NONE',  ( 232.4999999999996305, 133.0668745871126930, -36.86484227207694886 ) ) ;
#11781 = CARTESIAN_POINT ( 'NONE',  ( -144.7131007173674107, 126.7073428816716785, -16.81478254977324127 ) ) ;
#11782 = EDGE_CURVE ( 'NONE', #10524, #12184, #27365, .T. ) ;
#11783 = CARTESIAN_POINT ( 'NONE',  ( 79.99999999999995737, 93.29453619103988160, -96.96498881298317940 ) ) ;
#11784 = DIRECTION ( 'NONE',  ( 1.000000000000000000, 0.000000000000000000, 0.000000000000000000 ) ) ;
#11785 = VECTOR ( 'NONE', #5685, 1000.000000000000000 ) ;
#11786 = CARTESIAN_POINT ( 'NONE',  ( 158.0000000000000853, 198.9369999399436892, -45.00000000000000000 ) ) ;
#11787 = FACE_OUTER_BOUND ( 'NONE', #11293, .T. ) ;
#11788 = CARTESIAN_POINT ( 'NONE',  ( 93.07270601802888166, 112.9533406971467429, 74.06249999970600584 ) ) ;
#11789 = PRODUCT_RELATED_PRODUCT_CATEGORY ( 'part', '', ( #19684 ) ) ;
#11790 = FACE_OUTER_BOUND ( 'NONE', #10180, .T. ) ;
#11791 = CARTESIAN_POINT ( 'NONE',  ( -184.2178799556576791, 107.1030787669916435, 32.07408992895755517 ) ) ;
#11792 = LINE ( 'NONE', #22550, #1502 ) ;
#11794 = ORIENTED_EDGE ( 'NONE', *, *, #6271, .F. ) ;
#11793 = ORIENTED_EDGE ( 'NONE', *, *, #24931, .F. ) ;
#11795 = CARTESIAN_POINT ( 'NONE',  ( -218.6521670693695683, 86.22552751504353807, -19.45793375878209375 ) ) ;
#11796 = DIRECTION ( 'NONE',  ( 0.000000000000000000, 0.000000000000000000, -1.000000000000000000 ) ) ;
#11797 = ORIENTED_EDGE ( 'NONE', *, *, #13584, .F. ) ;
#11798 = CIRCLE ( 'NONE', #21405, 89.71075545852265520 ) ;
#11799 = ORIENTED_EDGE ( 'NONE', *, *, #27223, .T. ) ;
#11800 = DIRECTION ( 'NONE',  ( 1.000000000000000000, 0.000000000000000000, -0.000000000000000000 ) ) ;
#11801 = LINE ( 'NONE', #9637, #22778 ) ;
#11802 = ORIENTED_EDGE ( 'NONE', *, *, #2440, .T. ) ;
#11803 = VERTEX_POINT ( 'NONE', #3238 ) ;
#11804 = DIRECTION ( 'NONE',  ( 0.8916010070297749612, 0.4528218681374510668, 0.000000000000000000 ) ) ;
#11805 = FACE_OUTER_BOUND ( 'NONE', #15965, .T. ) ;
#11806 = EDGE_CURVE ( 'NONE', #2305, #12610, #954, .T. ) ;
#11807 = CARTESIAN_POINT ( 'NONE',  ( 157.4999999999998579, 60.74993702330277756, 45.00000000000000000 ) ) ;
#11808 = CARTESIAN_POINT ( 'NONE',  ( 134.9999999999998579, 220.0000000000000284, 100.0000000000000142 ) ) ;
#11809 = CARTESIAN_POINT ( 'NONE',  ( 134.9999999999998579, 404.6636166603179277, -138.9999999999999716 ) ) ;
#11810 = CYLINDRICAL_SURFACE ( 'NONE', #415, 30.00000000000000000 ) ;
#11811 = AXIS2_PLACEMENT_3D ( 'NONE', #18116, #13966, #22279 ) ;
#11812 = CARTESIAN_POINT ( 'NONE',  ( -214.2313421017086341, 58.42887478691789482, -32.84133050939110632 ) ) ;
#11813 = AXIS2_PLACEMENT_3D ( 'NONE', #8006, #20934, #14339 ) ;
#11814 = EDGE_CURVE ( 'NONE', #1235, #20045, #20361, .T. ) ;
#11815 = CARTESIAN_POINT ( 'NONE',  ( 158.0000000000007674, 133.2243747372535267, 45.00000000000000000 ) ) ;
#11816 = CARTESIAN_POINT ( 'NONE',  ( -180.0000000000000284, -40.00000000000004974, -25.00000000000000711 ) ) ;
#11817 = PLANE ( 'NONE',  #17085 ) ;
#11818 = DIRECTION ( 'NONE',  ( 1.000000000000000000, 0.000000000000000000, -0.000000000000000000 ) ) ;
#11819 = ORIENTED_EDGE ( 'NONE', *, *, #8251, .F. ) ;
#11820 = CARTESIAN_POINT ( 'NONE',  ( 294.9233831825460470, 127.6681916698403398, -145.0000000000000000 ) ) ;
#11821 = CARTESIAN_POINT ( 'NONE',  ( -234.0991496467403579, 66.75367139654557036, 6.159314286176283737 ) ) ;
#11822 = CARTESIAN_POINT ( 'NONE',  ( 124.9999999999998579, 220.0000000000000284, 90.00000000000002842 ) ) ;
#11823 = ORIENTED_EDGE ( 'NONE', *, *, #4349, .F. ) ;
#11824 = PRODUCT_CONTEXT ( 'NONE', #5981, 'mechanical' ) ;
#11825 = ORIENTED_EDGE ( 'NONE', *, *, #2690, .T. ) ;
#11826 = ADVANCED_FACE ( 'NONE', ( #3662 ), #25087, .F. ) ;
#11827 = EDGE_CURVE ( 'NONE', #22340, #7786, #22204, .T. ) ;
#11828 = CARTESIAN_POINT ( 'NONE',  ( 108.2273028572102760, 129.5338070841179672, 88.59375000028596503 ) ) ;
#11829 = CARTESIAN_POINT ( 'NONE',  ( -210.0000000000000284, 59.99999999999994316, 15.00000000000000000 ) ) ;
#11830 = ORIENTED_EDGE ( 'NONE', *, *, #23855, .F. ) ;
#11831 = AXIS2_PLACEMENT_3D ( 'NONE', #270, #15937, #13492 ) ;
#11832 = EDGE_LOOP ( 'NONE', ( #5173, #21341, #24786, #26354 ) ) ;
#11833 = CARTESIAN_POINT ( 'NONE',  ( -76.25760768171835480, 219.6666220619077876, -15.00000000000000000 ) ) ;
#11834 = LINE ( 'NONE', #18005, #23569 ) ;
#11835 = LINE ( 'NONE', #7655, #1330 ) ;
#11836 = ORIENTED_EDGE ( 'NONE', *, *, #1400, .T. ) ;
#11837 = DIRECTION ( 'NONE',  ( 0.9506505318133544602, 0.3102637045530566295, 0.000000000000000000 ) ) ;
#11838 = ORIENTED_EDGE ( 'NONE', *, *, #5323, .T. ) ;
#11839 = FACE_OUTER_BOUND ( 'NONE', #7855, .T. ) ;
#11840 = DIRECTION ( 'NONE',  ( -0.000000000000000000, -0.000000000000000000, -1.000000000000000000 ) ) ;
#11841 = DIRECTION ( 'NONE',  ( -0.000000000000000000, -0.000000000000000000, -1.000000000000000000 ) ) ;
#11842 = CARTESIAN_POINT ( 'NONE',  ( -28.20614712894950316, 129.1555222404294909, -15.69110854779580322 ) ) ;
#11843 = DIRECTION ( 'NONE',  ( 1.000000000000000000, 0.000000000000000000, 0.000000000000000000 ) ) ;
#11844 = EDGE_CURVE ( 'NONE', #18495, #21449, #18533, .T. ) ;
#11845 = CARTESIAN_POINT ( 'NONE',  ( -273.6138116763045787, -165.0000000000001990, -86.76535624830611937 ) ) ;
#11846 = CARTESIAN_POINT ( 'NONE',  ( 142.6536686473015152, 238.4775906502254941, 45.00000000000000000 ) ) ;
#11847 = VECTOR ( 'NONE', #12629, 1000.000000000000000 ) ;
#11848 = ORIENTED_EDGE ( 'NONE', *, *, #27692, .T. ) ;
#11849 = ADVANCED_FACE ( 'NONE', ( #27096 ), #23352, .F. ) ;
#11850 = CARTESIAN_POINT ( 'NONE',  ( 127.3463313526982716, 201.5224093497739943, 45.00000000000000000 ) ) ;
#11851 = CARTESIAN_POINT ( 'NONE',  ( -218.8273392347297488, 140.3457761587515336, 14.99191580167116911 ) ) ;
#11852 = DIRECTION ( 'NONE',  ( -0.000000000000000000, -1.000000000000000000, -0.000000000000000000 ) ) ;
#11853 = EDGE_LOOP ( 'NONE', ( #5767, #22873, #26835, #23118 ) ) ;
#11854 = CARTESIAN_POINT ( 'NONE',  ( 157.9999999999999432, 213.4763749774776045, -45.00000000000000000 ) ) ;
#11855 = EDGE_LOOP ( 'NONE', ( #17258, #4684, #14904, #2493 ) ) ;
#11856 = DIRECTION ( 'NONE',  ( -0.000000000000000000, -0.000000000000000000, -1.000000000000000000 ) ) ;
#11857 = CARTESIAN_POINT ( 'NONE',  ( 157.9999999999999432, 211.4763749774776045, 45.00000000000000000 ) ) ;
#11858 = DIRECTION ( 'NONE',  ( 0.000000000000000000, 0.000000000000000000, -1.000000000000000000 ) ) ;
#11859 = ORIENTED_EDGE ( 'NONE', *, *, #22561, .F. ) ;
#11860 = DIRECTION ( 'NONE',  ( 0.7440215159218921404, -0.6681556583950252204, 0.000000000000000000 ) ) ;
#11861 =( NAMED_UNIT ( * ) PLANE_ANGLE_UNIT ( ) SI_UNIT ( $, .RADIAN. ) );
#11862 = ORIENTED_EDGE ( 'NONE', *, *, #14327, .T. ) ;
#11863 = EDGE_CURVE ( 'NONE', #12495, #18743, #22355, .T. ) ;
#11864 = CARTESIAN_POINT ( 'NONE',  ( -75.15023727777021634, 134.4794526767016691, 15.51172362355055867 ) ) ;
#11865 = AXIS2_PLACEMENT_3D ( 'NONE', #9736, #22944, #22378 ) ;
#11866 = DIRECTION ( 'NONE',  ( -0.8916010070298056034, -0.4528218681373908372, 0.000000000000000000 ) ) ;
#11867 = ORIENTED_EDGE ( 'NONE', *, *, #10879, .T. ) ;
#11868 = EDGE_CURVE ( 'NONE', #13193, #11551, #21192, .T. ) ;
#11869 = ORIENTED_EDGE ( 'NONE', *, *, #13669, .T. ) ;
#11870 = EDGE_CURVE ( 'NONE', #4776, #9726, #23774, .T. ) ;
#11871 = LINE ( 'NONE', #20615, #9493 ) ;
#11872 = ORIENTED_EDGE ( 'NONE', *, *, #22390, .T. ) ;
#11873 = VECTOR ( 'NONE', #3520, 1000.000000000000000 ) ;
#11874 = AXIS2_PLACEMENT_3D ( 'NONE', #14698, #5504, #3342 ) ;
#11875 = EDGE_CURVE ( 'NONE', #3644, #7560, #25639, .T. ) ;
#11876 = ORIENTED_EDGE ( 'NONE', *, *, #3141, .F. ) ;
#11877 = ORIENTED_EDGE ( 'NONE', *, *, #9815, .F. ) ;
#11878 = CARTESIAN_POINT ( 'NONE',  ( 108.8501248000121109, 253.0299650810305536, 36.51570041463102001 ) ) ;
#11879 = APPLICATION_CONTEXT ( 'automotive_design' ) ;
#11880 = DIRECTION ( 'NONE',  ( -1.000000000000000000, -0.000000000000000000, -0.000000000000000000 ) ) ;
#11881 = LINE ( 'NONE', #5254, #14237 ) ;
#11882 = DIRECTION ( 'NONE',  ( 0.000000000000000000, -1.000000000000000000, 0.000000000000000000 ) ) ;
#11883 = CARTESIAN_POINT ( 'NONE',  ( 232.4999999999996305, 186.4134324495536248, -35.02193266779035952 ) ) ;
#11884 = DIRECTION ( 'NONE',  ( 0.7071067811865613395, 0.7071067811865336949, 0.000000000000000000 ) ) ;
#11885 = VECTOR ( 'NONE', #21115, 1000.000000000000000 ) ;
#11886 = CARTESIAN_POINT ( 'NONE',  ( 58.09044720719344213, 216.7965004116395562, 45.00000000000000000 ) ) ;
#11887 = DIRECTION ( 'NONE',  ( -0.8916010070300384172, 0.4528218681369324261, 0.000000000000000000 ) ) ;
#11888 = EDGE_CURVE ( 'NONE', #13449, #26259, #12872, .T. ) ;
#11889 = DIRECTION ( 'NONE',  ( 0.2759800118297804916, -0.9611633748070274041, 0.000000000000000000 ) ) ;
#11890 = CARTESIAN_POINT ( 'NONE',  ( 158.0000000000001990, 186.3976249024084666, 45.00000000000000000 ) ) ;
#11891 = CARTESIAN_POINT ( 'NONE',  ( 113.9305603607155888, 212.0895489533244245, -97.95022080735121506 ) ) ;
#11892 = ORIENTED_EDGE ( 'NONE', *, *, #13513, .T. ) ;
#11893 = VECTOR ( 'NONE', #2346, 1000.000000000000000 ) ;
#11894 = AXIS2_PLACEMENT_3D ( 'NONE', #24766, #18301, #7385 ) ;
#11895 = DIRECTION ( 'NONE',  ( 0.8516548651973804285, -0.5241030343220993704, 0.000000000000000000 ) ) ;
#11896 = FACE_OUTER_BOUND ( 'NONE', #14933, .T. ) ;
#11897 = FACE_OUTER_BOUND ( 'NONE', #2255, .T. ) ;
#11898 = ORIENTED_EDGE ( 'NONE', *, *, #11473, .F. ) ;
#11899 = VECTOR ( 'NONE', #1318, 999.9999999999998863 ) ;
#11900 = CARTESIAN_POINT ( 'NONE',  ( 65.00000000000000000, -170.0000000000000853, -75.99999999999997158 ) ) ;
#11901 = EDGE_LOOP ( 'NONE', ( #26393, #25660, #9603, #21159 ) ) ;
#11902 = FACE_OUTER_BOUND ( 'NONE', #16969, .T. ) ;
#11903 = ADVANCED_FACE ( 'NONE', ( #17302 ), #6530, .F. ) ;
#11904 = EDGE_LOOP ( 'NONE', ( #14370, #3929, #21484, #13605 ) ) ;
#11905 = EDGE_CURVE ( 'NONE', #26049, #15387, #23920, .T. ) ;
#11906 = VECTOR ( 'NONE', #22766, 1000.000000000000000 ) ;
#11907 = EDGE_CURVE ( 'NONE', #23339, #26492, #19463, .T. ) ;
#11908 = EDGE_LOOP ( 'NONE', ( #11667, #15745, #15033, #16073 ) ) ;
#11909 = EDGE_LOOP ( 'NONE', ( #5863, #15221, #27304, #16761 ) ) ;
#11910 = ORIENTED_EDGE ( 'NONE', *, *, #24532, .T. ) ;
#11911 = DIRECTION ( 'NONE',  ( 0.000000000000000000, -1.000000000000000000, 0.000000000000000000 ) ) ;
#11912 = PLANE ( 'NONE',  #10899 ) ;
#11913 = CARTESIAN_POINT ( 'NONE',  ( -211.4334854057310338, -220.0000000000001421, -92.30784275734241362 ) ) ;
#11914 = VECTOR ( 'NONE', #10040, 1000.000000000000000 ) ;
#11915 = CARTESIAN_POINT ( 'NONE',  ( -248.1546605714623013, -91.18033988749901653, 0.000000000000000000 ) ) ;
#11916 = DIRECTION ( 'NONE',  ( 0.000000000000000000, 0.000000000000000000, 1.000000000000000000 ) ) ;
#11917 = FACE_OUTER_BOUND ( 'NONE', #17407, .T. ) ;
#11918 = CARTESIAN_POINT ( 'NONE',  ( 158.0000000000008242, 126.2086247222394206, 45.00000000000000000 ) ) ;
#11919 = CARTESIAN_POINT ( 'NONE',  ( -151.7715828776752574, 124.0909716950949644, -18.38260046643562617 ) ) ;
#11920 = DIRECTION ( 'NONE',  ( 0.8660254037844432595, 0.4999999999999919509, -0.000000000000000000 ) ) ;
#11921 = DIRECTION ( 'NONE',  ( 0.8916010070293584056, 0.4528218681382713551, 0.000000000000000000 ) ) ;
#11922 = CARTESIAN_POINT ( 'NONE',  ( 232.4999999999996305, 133.0668745871126930, -36.86484227207694886 ) ) ;
#11923 = DIRECTION ( 'NONE',  ( -0.000000000000000000, -0.000000000000000000, -1.000000000000000000 ) ) ;
#11924 = CIRCLE ( 'NONE', #17415, 1.999999999999997335 ) ;
#11925 = CARTESIAN_POINT ( 'NONE',  ( 157.4999999999998579, 223.7618125112605298, -45.00000000000000000 ) ) ;
#11926 = VECTOR ( 'NONE', #7203, 1000.000000000000000 ) ;
#11927 = CARTESIAN_POINT ( 'NONE',  ( 104.4199312700659448, 89.58810137561040676, -100.0000000000000142 ) ) ;
#11928 = CARTESIAN_POINT ( 'NONE',  ( 158.0000000000007105, 136.2401247522676044, 45.00000000000000000 ) ) ;
#11929 = B_SPLINE_CURVE_WITH_KNOTS ( 'NONE', 3,
 ( #20172, #4504, #22043, #8974, #17305, #17731, #22332, #2641, #11427, #8557, #26478, #26065, #6808, #24631, #5229, #11993, #14288, #13872, #7674, #16304, #24777, #14149, #9412, #11574 ),
 .UNSPECIFIED., .F., .F.,
 ( 4, 2, 2, 2, 2, 2, 2, 2, 2, 2, 2, 4 ),
 ( 0.000000000000000000, 0.005275168248736577560, 0.007912752373104866774, 0.01055033649747315512, 0.01582550474620979947, 0.01846308887057816067, 0.02110067299494652188, 0.02637584124368318184, 0.02901342536805146324, 0.03165100949241975159, 0.03692617774115627971, 0.04220134598989280783 ),
 .UNSPECIFIED. ) ;
#11931 = ORIENTED_EDGE ( 'NONE', *, *, #2793, .F. ) ;
#11930 = VERTEX_POINT ( 'NONE', #6107 ) ;
#11932 = VECTOR ( 'NONE', #14892, 1000.000000000000000 ) ;
#11933 = LINE ( 'NONE', #1276, #18004 ) ;
#11934 = VERTEX_POINT ( 'NONE', #1652 ) ;
#11936 = ORIENTED_EDGE ( 'NONE', *, *, #8822, .T. ) ;
#11935 = AXIS2_PLACEMENT_3D ( 'NONE', #5711, #14484, #5989 ) ;
#11937 = EDGE_CURVE ( 'NONE', #16168, #6585, #21334, .T. ) ;
#11938 = LINE ( 'NONE', #2582, #6080 ) ;
#11939 = ADVANCED_FACE ( 'NONE', ( #10423 ), #24030, .T. ) ;
#11940 = VERTEX_POINT ( 'NONE', #3946 ) ;
#11941 = ORIENTED_EDGE ( 'NONE', *, *, #5398, .F. ) ;
#11942 = DIRECTION ( 'NONE',  ( 0.000000000000000000, 1.000000000000000000, -0.000000000000000000 ) ) ;
#11943 = DIRECTION ( 'NONE',  ( 1.000000000000000000, 0.000000000000000000, 0.000000000000000000 ) ) ;
#11944 = AXIS2_PLACEMENT_3D ( 'NONE', #16742, #21462, #21181 ) ;
#11945 = DIRECTION ( 'NONE',  ( 1.000000000000000000, 0.000000000000000000, 0.000000000000000000 ) ) ;
#11946 = CARTESIAN_POINT ( 'NONE',  ( 95.56988606615753667, 231.9897823149801752, -19.35215035236615932 ) ) ;
#11947 = CIRCLE ( 'NONE', #7366, 79.71075545852265520 ) ;
#11948 = CARTESIAN_POINT ( 'NONE',  ( 367.4999999999996021, 44.41075299063184900, 1.850330238640837654E-14 ) ) ;
#11949 = CARTESIAN_POINT ( 'NONE',  ( 113.4999999999998863, 220.0000000000000284, -99.00000000000001421 ) ) ;
#11950 = CARTESIAN_POINT ( 'NONE',  ( -217.0794644928006392, 71.41167302539398065, -24.35665452625710259 ) ) ;
#11951 = CARTESIAN_POINT ( 'NONE',  ( 111.4893267626885205, 201.3648822632117117, -149.1019530262190358 ) ) ;
#11952 = DIRECTION ( 'NONE',  ( 0.000000000000000000, 1.024644424698391667E-16, -1.000000000000000000 ) ) ;
#11953 = DIRECTION ( 'NONE',  ( 1.000000000000000000, 0.000000000000000000, -0.000000000000000000 ) ) ;
#11954 = DIRECTION ( 'NONE',  ( 0.000000000000000000, 0.000000000000000000, 1.000000000000000000 ) ) ;
#11955 = VERTEX_POINT ( 'NONE', #14887 ) ;
#11956 = FACE_OUTER_BOUND ( 'NONE', #14353, .T. ) ;
#11957 = EDGE_CURVE ( 'NONE', #12076, #15277, #23637, .T. ) ;
#11958 = VECTOR ( 'NONE', #3197, 1000.000000000000000 ) ;
#11959 = CARTESIAN_POINT ( 'NONE',  ( -235.2766700735673169, 67.45978041260606517, 15.24953891110985182 ) ) ;
#11960 = CARTESIAN_POINT ( 'NONE',  ( 157.4999999999998579, 146.0176872785422404, 45.00000000000000000 ) ) ;
#11961 = ORIENTED_EDGE ( 'NONE', *, *, #24650, .T. ) ;
#11962 = CARTESIAN_POINT ( 'NONE',  ( -175.0000000000000000, -114.0000000000001847, -69.99999999999998579 ) ) ;
#11963 = SHAPE_REPRESENTATION ( 'MAS-315', ( #1012, #9273, #26232, #94, #16173, #1462, #17519, #16613, #6057, #26707, #5139, #3751, #28067, #27594, #24418 ), #14788 ) ;
#11964 = VERTEX_POINT ( 'NONE', #8124 ) ;
#11965 = VECTOR ( 'NONE', #2603, 1000.000000000000000 ) ;
#11966 = CARTESIAN_POINT ( 'NONE',  ( 101.7779539752123981, 119.2876405402088835, 100.0000000000000142 ) ) ;
#11967 = LINE ( 'NONE', #14261, #25979 ) ;
#11968 = EDGE_CURVE ( 'NONE', #10398, #18134, #21472, .T. ) ;
#11969 = ORIENTED_EDGE ( 'NONE', *, *, #13521, .T. ) ;
#11970 = ORIENTED_EDGE ( 'NONE', *, *, #7918, .F. ) ;
#11971 = CARTESIAN_POINT ( 'NONE',  ( 157.9999999999996874, 264.1417501351260171, 45.00000000000000000 ) ) ;
#11972 = EDGE_CURVE ( 'NONE', #26778, #14369, #19320, .T. ) ;
#11973 = CARTESIAN_POINT ( 'NONE',  ( 157.4999999999998579, 60.74993702330277756, 45.00000000000000000 ) ) ;
#11974 = DIRECTION ( 'NONE',  ( 0.8379557447115515423, -0.5457381880580733924, 0.000000000000000000 ) ) ;
#11975 = ORIENTED_EDGE ( 'NONE', *, *, #10666, .T. ) ;
#11976 = DIRECTION ( 'NONE',  ( 0.000000000000000000, -1.000000000000000000, 0.000000000000000000 ) ) ;
#11977 = ORIENTED_EDGE ( 'NONE', *, *, #17402, .F. ) ;
#11978 = LINE ( 'NONE', #24901, #25376 ) ;
#11979 = VECTOR ( 'NONE', #26164, 1000.000000000000000 ) ;
#11980 = DIRECTION ( 'NONE',  ( 0.000000000000000000, 0.000000000000000000, -1.000000000000000000 ) ) ;
#11981 = LINE ( 'NONE', #5355, #16280 ) ;
#11982 = CARTESIAN_POINT ( 'NONE',  ( -38.26643717395023003, 130.0143911579998530, -16.67725966943145366 ) ) ;
#11983 = LINE ( 'NONE', #26775, #10033 ) ;
#11984 = ADVANCED_FACE ( 'NONE', ( #15022 ), #636, .F. ) ;
#11985 = CARTESIAN_POINT ( 'NONE',  ( -207.5617036789550980, 75.42459176675926358, -44.71595801440848561 ) ) ;
#11986 = VECTOR ( 'NONE', #12697, 1000.000000000000227 ) ;
#11987 = CARTESIAN_POINT ( 'NONE',  ( 349.0018770490533484, 96.44595867864246941, -145.0000000000000000 ) ) ;
#11988 = ORIENTED_EDGE ( 'NONE', *, *, #16810, .T. ) ;
#11989 = LINE ( 'NONE', #18582, #1287 ) ;
#11990 = CYLINDRICAL_SURFACE ( 'NONE', #17068, 5.999999999999991118 ) ;
#11991 = DIRECTION ( 'NONE',  ( -0.000000000000000000, -0.000000000000000000, 1.000000000000000000 ) ) ;
#11992 = ORIENTED_EDGE ( 'NONE', *, *, #12906, .F. ) ;
#11993 = CARTESIAN_POINT ( 'NONE',  ( -233.4149848405407681, 66.33036726544320061, 6.308275885109302372 ) ) ;
#11994 = ORIENTED_EDGE ( 'NONE', *, *, #11844, .F. ) ;
#11995 = EDGE_CURVE ( 'NONE', #23684, #8916, #8828, .T. ) ;
#11996 = FACE_OUTER_BOUND ( 'NONE', #25506, .T. ) ;
#11997 = LINE ( 'NONE', #20885, #943 ) ;
#11998 = CARTESIAN_POINT ( 'NONE',  ( 134.9999999999998579, 250.0000000000000568, -138.9999999999999432 ) ) ;
#11999 = EDGE_LOOP ( 'NONE', ( #920, #12962, #4696, #3484 ) ) ;
#12000 = DIRECTION ( 'NONE',  ( -1.000000000000000000, 0.000000000000000000, 3.097027491608645765E-15 ) ) ;
#12001 = ORIENTED_EDGE ( 'NONE', *, *, #25282, .F. ) ;
#12002 = AXIS2_PLACEMENT_3D ( 'NONE', #11315, #22511, #10884 ) ;
#12003 = CARTESIAN_POINT ( 'NONE',  ( -86.44332993818018451, 134.8061491223789972, 15.45302073408354993 ) ) ;
#12004 = CARTESIAN_POINT ( 'NONE',  ( 108.2138036696523642, 251.6610875895352137, 30.47597920753440803 ) ) ;
#12005 = ORIENTED_EDGE ( 'NONE', *, *, #5266, .T. ) ;
#12006 = ORIENTED_EDGE ( 'NONE', *, *, #14096, .F. ) ;
#12007 = CARTESIAN_POINT ( 'NONE',  ( -143.6428522700808230, 20.24192588826928585, 80.00000000000001421 ) ) ;
#12008 = ORIENTED_EDGE ( 'NONE', *, *, #25783, .T. ) ;
#12009 = CIRCLE ( 'NONE', #53, 5.999999999999977796 ) ;
#12010 = EDGE_CURVE ( 'NONE', #3702, #22223, #11572, .T. ) ;
#12011 = EDGE_CURVE ( 'NONE', #26013, #15680, #21899, .T. ) ;
#12012 = ORIENTED_EDGE ( 'NONE', *, *, #26997, .F. ) ;
#12013 = VERTEX_POINT ( 'NONE', #26475 ) ;
#12014 = DIRECTION ( 'NONE',  ( 0.8916010070297244461, 0.4528218681375507093, 0.000000000000000000 ) ) ;
#12015 = CARTESIAN_POINT ( 'NONE',  ( 187.4999999999996305, 133.0668745871126930, -36.86484227207694886 ) ) ;
#12016 = CARTESIAN_POINT ( 'NONE',  ( -229.2498027451139251, 132.0565166830976693, 15.00000000000000000 ) ) ;
#12017 = EDGE_CURVE ( 'NONE', #24036, #9050, #19741, .T. ) ;
#12018 = CARTESIAN_POINT ( 'NONE',  ( 94.38583646783695258, 113.6320904521875548, -75.15625000023771918 ) ) ;
#12019 = CARTESIAN_POINT ( 'NONE',  ( 158.0000000000004263, 166.3346248423521274, 45.00000000000000000 ) ) ;
#12020 = CARTESIAN_POINT ( 'NONE',  ( 157.4999999999998579, 141.0019372635281627, 45.00000000000000000 ) ) ;
#12021 = EDGE_CURVE ( 'NONE', #230, #22407, #6590, .T. ) ;
#12022 = VECTOR ( 'NONE', #6493, 1000.000000000000000 ) ;
#12023 = CARTESIAN_POINT ( 'NONE',  ( 109.9999999999999432, -100.0000000000000142, 70.00000000000001421 ) ) ;
#12024 = CARTESIAN_POINT ( 'NONE',  ( -266.6333112347296606, -170.8236892866178209, 104.6429431552469111 ) ) ;
#12026 = DIRECTION ( 'NONE',  ( 0.4528218681382319422, 0.8916010070293783896, -0.000000000000000000 ) ) ;
#12025 = CIRCLE ( 'NONE', #16171, 10.00000000000000888 ) ;
#12027 = DIRECTION ( 'NONE',  ( -1.000000000000000000, -1.321694076934710155E-16, 0.000000000000000000 ) ) ;
#12028 = MECHANICAL_DESIGN_GEOMETRIC_PRESENTATION_REPRESENTATION (  '', ( #7428 ), #15222 ) ;
#12029 = ORIENTED_EDGE ( 'NONE', *, *, #22633, .F. ) ;
#12030 = EDGE_CURVE ( 'NONE', #2218, #19998, #27679, .T. ) ;
#12031 = AXIS2_PLACEMENT_3D ( 'NONE', #27101, #20639, #27238 ) ;
#12032 = CARTESIAN_POINT ( 'NONE',  ( 157.4999999999998579, 168.5885623461056184, 45.00000000000000000 ) ) ;
#12033 = DIRECTION ( 'NONE',  ( -0.5457381880580733924, -0.8379557447115515423, 0.000000000000000000 ) ) ;
#12034 = EDGE_CURVE ( 'NONE', #9697, #14502, #7102, .T. ) ;
#12035 = DIRECTION ( 'NONE',  ( -1.000000000000000000, 0.000000000000000000, -2.775557561562887407E-16 ) ) ;
#12036 = DIRECTION ( 'NONE',  ( 0.8916010070293409751, 0.4528218681383056610, 0.000000000000000000 ) ) ;
#12037 = ORIENTED_EDGE ( 'NONE', *, *, #14838, .T. ) ;
#12038 = CARTESIAN_POINT ( 'NONE',  ( 134.9999999999998579, 220.0000000000000284, 90.00000000000002842 ) ) ;
#12039 = EDGE_LOOP ( 'NONE', ( #15955, #15454, #9550, #25542 ) ) ;
#12040 = LINE ( 'NONE', #547, #1806 ) ;
#12041 = ORIENTED_EDGE ( 'NONE', *, *, #7692, .T. ) ;
#12042 = B_SPLINE_CURVE_WITH_KNOTS ( 'NONE', 3,
 ( #8627, #6609, #17377, #17099, #2427, #24275, #4445, #13230, #26140, #6464, #8912, #295, #13660, #5165, #20394, #11795, #26996, #5016, #6890, #9198, #24419, #20533, #15820, #22700, #724, #7038, #2865, #2574, #16101, #11655 ),
 .UNSPECIFIED., .F., .F.,
 ( 4, 2, 2, 2, 2, 2, 2, 2, 2, 2, 2, 2, 2, 2, 4 ),
 ( 1.076317285288624681E-15, 0.002329614659891489793, 0.003494421989836663748, 0.004659229319781837270, 0.009318458639562503601, 0.01164807329945279947, 0.01397768795934309534, 0.01630730261923338947, 0.01863691727912368534, 0.02329614659890428055, 0.02795537591868487923, 0.03028499057857521326, 0.03261460523846554382, 0.03494421989835588827, 0.03727383455824621883 ),
 .UNSPECIFIED. ) ;
#12043 = ORIENTED_EDGE ( 'NONE', *, *, #9629, .F. ) ;
#12044 = AXIS2_PLACEMENT_3D ( 'NONE', #3164, #20131, #2893 ) ;
#12045 = EDGE_LOOP ( 'NONE', ( #22347, #23303, #20965, #10271 ) ) ;
#12046 = ORIENTED_EDGE ( 'NONE', *, *, #12188, .F. ) ;
#12047 = ORIENTED_EDGE ( 'NONE', *, *, #23294, .F. ) ;
#12048 = AXIS2_PLACEMENT_3D ( 'NONE', #5023, #22563, #9636 ) ;
#12049 = DIRECTION ( 'NONE',  ( 1.000000000000000000, 0.000000000000000000, 0.000000000000000000 ) ) ;
#12050 = FACE_OUTER_BOUND ( 'NONE', #21751, .T. ) ;
#12051 = DIRECTION ( 'NONE',  ( -1.000000000000000000, 0.000000000000000000, -0.000000000000000000 ) ) ;
#12052 = AXIS2_PLACEMENT_3D ( 'NONE', #13302, #20180, #10858 ) ;
#12053 = LINE ( 'NONE', #27118, #8246 ) ;
#12054 = LINE ( 'NONE', #18646, #16703 ) ;
#12055 = CARTESIAN_POINT ( 'NONE',  ( 134.9999999999998863, 537.6859242279716682, -145.0000000000000000 ) ) ;
#12056 = CARTESIAN_POINT ( 'NONE',  ( 113.0425250404539241, 213.0812361363525440, 45.00000000000000000 ) ) ;
#12057 = CARTESIAN_POINT ( 'NONE',  ( 157.4999999999998579, 118.4310621959647563, 45.00000000000000000 ) ) ;
#12058 = DIRECTION ( 'NONE',  ( 1.000000000000000000, 0.000000000000000000, 0.000000000000000000 ) ) ;
#12059 = CARTESIAN_POINT ( 'NONE',  ( -219.0853371859187746, 87.86960372567372701, -16.90895988174265696 ) ) ;
#12060 = EDGE_CURVE ( 'NONE', #9244, #18948, #15883, .T. ) ;
#12061 = DIRECTION ( 'NONE',  ( 0.000000000000000000, 0.000000000000000000, -1.000000000000000000 ) ) ;
#12062 = CARTESIAN_POINT ( 'NONE',  ( -66.26041567618258910, 130.4659900502583127, 45.00000000000000000 ) ) ;
#12063 = LINE ( 'NONE', #20811, #5198 ) ;
#12064 = VERTEX_POINT ( 'NONE', #16021 ) ;
#12065 = VECTOR ( 'NONE', #557, 1000.000000000000114 ) ;
#12066 = EDGE_CURVE ( 'NONE', #17060, #7044, #9355, .T. ) ;
#12067 = TOROIDAL_SURFACE ( 'NONE', #24410, 68.83858790703926900, 2.000000000000000000 ) ;
#12068 = CARTESIAN_POINT ( 'NONE',  ( 367.9108539694884144, 44.41075299063183479, 100.0000000000000284 ) ) ;
#12069 = LINE ( 'NONE', #19180, #9780 ) ;
#12070 = VECTOR ( 'NONE', #20664, 1000.000000000000000 ) ;
#12072 = ORIENTED_EDGE ( 'NONE', *, *, #3569, .T. ) ;
#12071 = VERTEX_POINT ( 'NONE', #65 ) ;
#12073 = AXIS2_PLACEMENT_3D ( 'NONE', #2867, #24421, #4730 ) ;
#12074 = CARTESIAN_POINT ( 'NONE',  ( 157.9999999999998863, 216.4921249924925348, -45.00000000000000000 ) ) ;
#12075 = ORIENTED_EDGE ( 'NONE', *, *, #7614, .F. ) ;
#12076 = VERTEX_POINT ( 'NONE', #2638 ) ;
#12077 = VERTEX_POINT ( 'NONE', #24199 ) ;
#12078 = ORIENTED_EDGE ( 'NONE', *, *, #7288, .T. ) ;
#12079 = ORIENTED_EDGE ( 'NONE', *, *, #11069, .T. ) ;
#12080 = LINE ( 'NONE', #20827, #2023 ) ;
#12081 = VECTOR ( 'NONE', #5951, 1000.000000000000114 ) ;
#12082 = CARTESIAN_POINT ( 'NONE',  ( 100.0000000000004974, -280.0000000000000000, 209.9999999999999716 ) ) ;
#12083 = AXIS2_PLACEMENT_3D ( 'NONE', #4937, #26348, #11430 ) ;
#12084 = EDGE_CURVE ( 'NONE', #21404, #13671, #17874, .T. ) ;
#12085 = CARTESIAN_POINT ( 'NONE',  ( -189.8086322075389774, 92.49158130768422836, -13.00000000000000000 ) ) ;
#12086 = AXIS2_PLACEMENT_3D ( 'NONE', #15347, #25818, #24103 ) ;
#12087 = FACE_OUTER_BOUND ( 'NONE', #23266, .T. ) ;
#12088 = VECTOR ( 'NONE', #20501, 1000.000000000000000 ) ;
#12089 = FACE_BOUND ( 'NONE', #8511, .T. ) ;
#12090 = LINE ( 'NONE', #740, #8946 ) ;
#12091 = EDGE_CURVE ( 'NONE', #12823, #4413, #4501, .T. ) ;
#12092 = DIRECTION ( 'NONE',  ( -0.8916010070296226386, -0.4528218681377511046, 0.000000000000000000 ) ) ;
#12093 = DIRECTION ( 'NONE',  ( 0.9960550913260673989, 0.000000000000000000, -0.08873699929240025375 ) ) ;
#12094 = EDGE_CURVE ( 'NONE', #2548, #7910, #22474, .T. ) ;
#12095 = EDGE_CURVE ( 'NONE', #10355, #12452, #8446, .T. ) ;
#12096 = CARTESIAN_POINT ( 'NONE',  ( 111.2276402061722109, 201.6982782665056675, -140.4786076439499425 ) ) ;
#12097 = EDGE_CURVE ( 'NONE', #11940, #23711, #2489, .T. ) ;
#12098 = CARTESIAN_POINT ( 'NONE',  ( 179.9999999999999147, 0.000000000000000000, 100.0000000000000142 ) ) ;
#12099 = CARTESIAN_POINT ( 'NONE',  ( 158.0000000000009663, 115.6692496847042264, -45.00000000000000000 ) ) ;
#12100 = CARTESIAN_POINT ( 'NONE',  ( 134.1167547769962596, -7.205103435269982093, 45.00000000000000000 ) ) ;
#12101 = ORIENTED_EDGE ( 'NONE', *, *, #3517, .T. ) ;
#12102 = VECTOR ( 'NONE', #14099, 1000.000000000000114 ) ;
#12103 = CARTESIAN_POINT ( 'NONE',  ( -192.3996610505091951, 101.6547306301078493, 31.99652495868150837 ) ) ;
#12104 = CARTESIAN_POINT ( 'NONE',  ( 158.0000000000004832, 163.3188748273380213, -45.00000000000000000 ) ) ;
#12105 = EDGE_LOOP ( 'NONE', ( #11910, #4231, #12955, #24887 ) ) ;
#12106 = DIRECTION ( 'NONE',  ( -1.387778780781445429E-16, 1.387778780781445429E-16, 1.000000000000000000 ) ) ;
#12107 = CIRCLE ( 'NONE', #7049, 30.00000000000000000 ) ;
#12108 = ORIENTED_EDGE ( 'NONE', *, *, #14326, .T. ) ;
#12109 = ORIENTED_EDGE ( 'NONE', *, *, #18044, .T. ) ;
#12110 = LINE ( 'NONE', #13842, #8804 ) ;
#12111 = CARTESIAN_POINT ( 'NONE',  ( 157.9999999999997158, 258.6181251126050711, 45.00000000000000000 ) ) ;
#12112 = ORIENTED_EDGE ( 'NONE', *, *, #22353, .F. ) ;
#12113 = VERTEX_POINT ( 'NONE', #9409 ) ;
#12114 = LINE ( 'NONE', #3743, #21425 ) ;
#12115 = DIRECTION ( 'NONE',  ( 0.000000000000000000, -1.000000000000000000, 0.000000000000000000 ) ) ;
#12116 = CARTESIAN_POINT ( 'NONE',  ( 158.0000000000016200, 52.97237449702815582, -45.00000000000000000 ) ) ;
#12117 = ORIENTED_EDGE ( 'NONE', *, *, #12806, .F. ) ;
#12118 = CARTESIAN_POINT ( 'NONE',  ( -229.8316118350242334, 91.76664267010038145, 15.14942932049869917 ) ) ;
#12119 = EDGE_LOOP ( 'NONE', ( #25853, #23053, #28182, #1766 ) ) ;
#12120 = AXIS2_PLACEMENT_3D ( 'NONE', #19946, #2556, #8893 ) ;
#12121 = DIRECTION ( 'NONE',  ( -0.000000000000000000, -0.000000000000000000, 1.000000000000000000 ) ) ;
#12122 = EDGE_CURVE ( 'NONE', #4186, #21416, #20313, .T. ) ;
#12123 = ADVANCED_FACE ( 'NONE', ( #18171 ), #4791, .T. ) ;
#12124 = CARTESIAN_POINT ( 'NONE',  ( 158.0000000000014779, 65.51174953456337846, -45.00000000000000000 ) ) ;
#12125 = DIRECTION ( 'NONE',  ( 0.000000000000000000, 1.000000000000000000, 0.000000000000000000 ) ) ;
#12126 = DIRECTION ( 'NONE',  ( -0.8916010070293584056, -0.4528218681382712996, 0.000000000000000000 ) ) ;
#12127 = VECTOR ( 'NONE', #12558, 1000.000000000000000 ) ;
#12128 = DIRECTION ( 'NONE',  ( 0.000000000000000000, 0.000000000000000000, 1.000000000000000000 ) ) ;
#12129 = CARTESIAN_POINT ( 'NONE',  ( -17.24491960465747553, 29.64876300893806516, 100.0000000000000000 ) ) ;
#12130 = CARTESIAN_POINT ( 'NONE',  ( -199.1824292897938449, 96.09958175297150262, -31.38469581239659334 ) ) ;
#12131 = VERTEX_POINT ( 'NONE', #2347 ) ;
#12132 = CARTESIAN_POINT ( 'NONE',  ( 158.0000000000013074, 81.06687458711267880, 45.00000000000000000 ) ) ;
#12133 = EDGE_CURVE ( 'NONE', #21744, #14063, #2922, .T. ) ;
#12134 =( BOUNDED_SURFACE ( )  B_SPLINE_SURFACE ( 3, 2, ( 
 ( #3545, #6136, #27951 ),
 ( #12337, #27671, #5849 ),
 ( #21647, #14912, #14620 ),
 ( #10591, #23666, #23378 ),
 ( #25667, #14767, #3972 ),
 ( #21498, #12478, #3686 ),
 ( #21219, #1817, #10308 ),
 ( #5712, #21079, #19067 ),
 ( #1957, #19347, #10740 ),
 ( #25954, #28096, #8440 ),
 ( #4115, #5990, #28237 ),
 ( #19494, #8582, #23519 ) ),
 .UNSPECIFIED., .F., .F., .T. ) 
 B_SPLINE_SURFACE_WITH_KNOTS ( ( 4, 2, 2, 2, 2, 4 ),
 ( 3, 3 ),
 ( 0.000000000000000000, 0.004509347248874698982, 0.009018694497749397965, 0.01127336812218674746, 0.01352804174662409695, 0.01803738899549879593 ),
 ( 0.000000000000000000, 1.000000000000000000 ),
 .UNSPECIFIED. ) 
 GEOMETRIC_REPRESENTATION_ITEM ( )  RATIONAL_B_SPLINE_SURFACE ( (
 ( 1.000000000000000000, 0.7071067811865466846, 1.000000000000000000),
 ( 1.000000000000000000, 0.7039097745451907695, 1.000000000000000000),
 ( 1.000000000000000000, 0.7013522928558304503, 1.000000000000000000),
 ( 1.000000000000000000, 0.6977882347214663383, 1.000000000000000000),
 ( 1.000000000000000000, 0.6967820801478910031, 1.000000000000000000),
 ( 1.000000000000000000, 0.6966221438781953212, 1.000000000000000000),
 ( 1.000000000000000000, 0.6967948695995229702, 1.000000000000000000),
 ( 1.000000000000000000, 0.6976115817203014657, 1.000000000000000000),
 ( 1.000000000000000000, 0.6982527460775038719, 1.000000000000000000),
 ( 1.000000000000000000, 0.7008698237985928614, 1.000000000000000000),
 ( 1.000000000000000000, 0.7035399889988015465, 1.000000000000000000),
 ( 1.000000000000000000, 0.7071067811865475727, 1.000000000000000000) ) ) 
 REPRESENTATION_ITEM ( '' )  SURFACE ( )  );
#12135 = CARTESIAN_POINT ( 'NONE',  ( 158.0000000000005684, 153.2873747973098659, 45.00000000000000000 ) ) ;
#12136 = CARTESIAN_POINT ( 'NONE',  ( -217.6530433929989101, 140.9974892713794929, 15.00000000000000000 ) ) ;
#12137 = CARTESIAN_POINT ( 'NONE',  ( -260.0000000000001137, -157.0000000000000284, 60.00000000000002132 ) ) ;
#12138 = ORIENTED_EDGE ( 'NONE', *, *, #10817, .T. ) ;
#12139 = FACE_OUTER_BOUND ( 'NONE', #16105, .T. ) ;
#12140 = ORIENTED_EDGE ( 'NONE', *, *, #9465, .T. ) ;
#12141 = EDGE_CURVE ( 'NONE', #20397, #1420, #24775, .T. ) ;
#12142 = CARTESIAN_POINT ( 'NONE',  ( 157.9999999999999716, 210.9684999699701393, 45.00000000000000000 ) ) ;
#12143 = DIRECTION ( 'NONE',  ( -0.000000000000000000, -0.000000000000000000, -1.000000000000000000 ) ) ;
#12144 = CARTESIAN_POINT ( 'NONE',  ( 372.9108539694884144, -5.589247009368157215, 74.80456309157131045 ) ) ;
#12145 = ORIENTED_EDGE ( 'NONE', *, *, #2049, .T. ) ;
#12146 = DIRECTION ( 'NONE',  ( -0.000000000000000000, 0.000000000000000000, -1.000000000000000000 ) ) ;
#12147 = CARTESIAN_POINT ( 'NONE',  ( 144.9999999999998863, 220.0000000000000284, 90.00000000000002842 ) ) ;
#12148 = VERTEX_POINT ( 'NONE', #18309 ) ;
#12149 = TOROIDAL_SURFACE ( 'NONE', #25898, 16.91094714394370158, 6.204828372381208546 ) ;
#12150 = CARTESIAN_POINT ( 'NONE',  ( -248.1546605714623013, -91.18033988749901653, 16.91094714394370158 ) ) ;
#12151 = FACE_OUTER_BOUND ( 'NONE', #9873, .T. ) ;
#12152 = ORIENTED_EDGE ( 'NONE', *, *, #25843, .T. ) ;
#12153 = VECTOR ( 'NONE', #15415, 1000.000000000000227 ) ;
#12154 = ORIENTED_EDGE ( 'NONE', *, *, #13897, .T. ) ;
#12155 = CARTESIAN_POINT ( 'NONE',  ( 140.5127944162910865, 243.3752990424897575, 45.00000000000000000 ) ) ;
#12156 = ORIENTED_EDGE ( 'NONE', *, *, #25981, .F. ) ;
#12157 = EDGE_LOOP ( 'NONE', ( #27025, #5869, #17076, #4543 ) ) ;
#12158 = ORIENTED_EDGE ( 'NONE', *, *, #1590, .F. ) ;
#12159 = CARTESIAN_POINT ( 'NONE',  ( 109.9730600663563393, 258.3045051371393015, 43.53165882722885982 ) ) ;
#12160 = EDGE_CURVE ( 'NONE', #14719, #20334, #27469, .T. ) ;
#12161 = CARTESIAN_POINT ( 'NONE',  ( 0.000000000000000000, 0.000000000000000000, -25.00000000000000000 ) ) ;
#12162 = CARTESIAN_POINT ( 'NONE',  ( -80.45020005564978760, 95.60976900091465325, -145.0000000000000000 ) ) ;
#12163 = VECTOR ( 'NONE', #2561, 1000.000000000000114 ) ;
#12164 = DIRECTION ( 'NONE',  ( -0.8916010070293995948, -0.4528218681381900867, 0.000000000000000000 ) ) ;
#12165 = LINE ( 'NONE', #3091, #23200 ) ;
#12166 = CARTESIAN_POINT ( 'NONE',  ( 157.9999999999997726, 248.5866250825770294, 45.00000000000000000 ) ) ;
#12167 = DIRECTION ( 'NONE',  ( 0.000000000000000000, 9.251858538542967883E-17, -1.000000000000000000 ) ) ;
#12168 = AXIS2_PLACEMENT_3D ( 'NONE', #10856, #8560, #17309 ) ;
#12169 = CARTESIAN_POINT ( 'NONE',  ( -266.4957295474704893, -165.8849619812661444, 109.6032701725642937 ) ) ;
#12170 = DIRECTION ( 'NONE',  ( 1.000000000000000000, 0.000000000000000000, -1.224646799147353207E-16 ) ) ;
#12171 = PLANE ( 'NONE',  #26751 ) ;
#12172 = VERTEX_POINT ( 'NONE', #20595 ) ;
#12173 = CARTESIAN_POINT ( 'NONE',  ( -11.05879453184508421, 130.1926234397373605, 16.63927220650600702 ) ) ;
#12174 = EDGE_CURVE ( 'NONE', #2119, #2123, #3346, .T. ) ;
#12175 = EDGE_CURVE ( 'NONE', #1568, #11551, #21012, .T. ) ;
#12176 = CARTESIAN_POINT ( 'NONE',  ( 102.7211314862593099, 244.5532733014852909, -17.51403904043078441 ) ) ;
#12177 = CARTESIAN_POINT ( 'NONE',  ( 25.96679874230557061, 85.42000967830594504, 99.51128369927819506 ) ) ;
#12178 = CARTESIAN_POINT ( 'NONE',  ( 158.0000000000015348, 60.49599951954928656, 45.00000000000000000 ) ) ;
#12179 = B_SPLINE_CURVE_WITH_KNOTS ( 'NONE', 3,
 ( #6987, #26373, #24517, #388, #22075, #28374, #10882 ),
 .UNSPECIFIED., .F., .F.,
 ( 4, 3, 4 ),
 ( 0.01279859917594709795, 0.01395283628746606976, 0.01484145024773120096 ),
 .UNSPECIFIED. ) ;
#12180 = VERTEX_POINT ( 'NONE', #27060 ) ;
#12181 = DIRECTION ( 'NONE',  ( 0.000000000000000000, 0.000000000000000000, 1.000000000000000000 ) ) ;
#12182 = ORIENTED_EDGE ( 'NONE', *, *, #27695, .T. ) ;
#12183 = DIRECTION ( 'NONE',  ( 1.000000000000000000, 0.000000000000000000, 0.000000000000000000 ) ) ;
#12184 = VERTEX_POINT ( 'NONE', #7394 ) ;
#12185 = CIRCLE ( 'NONE', #8944, 10.53396790234563518 ) ;
#12186 = VECTOR ( 'NONE', #4823, 1000.000000000000000 ) ;
#12187 = AXIS2_PLACEMENT_3D ( 'NONE', #27658, #1527, #16764 ) ;
#12188 = EDGE_CURVE ( 'NONE', #4667, #13173, #22764, .T. ) ;
#12189 = VERTEX_POINT ( 'NONE', #23179 ) ;
#12190 = ADVANCED_FACE ( 'NONE', ( #5227 ), #27239, .F. ) ;
#12191 = EDGE_LOOP ( 'NONE', ( #4323, #11064, #28146, #19258 ) ) ;
#12192 = AXIS2_PLACEMENT_3D ( 'NONE', #6499, #25607, #1623 ) ;
#12193 = EDGE_LOOP ( 'NONE', ( #13987, #6161 ) ) ;
#12194 = CARTESIAN_POINT ( 'NONE',  ( 115.1311745403714326, 209.3942962959461056, 98.75303131641565813 ) ) ;
#12195 = LINE ( 'NONE', #24969, #15043 ) ;
#12196 = PLANE ( 'NONE',  #13916 ) ;
#12197 = CARTESIAN_POINT ( 'NONE',  ( -82.59029360989333668, 136.4857614611269412, -15.15915259372811619 ) ) ;
#12198 = DIRECTION ( 'NONE',  ( -0.000000000000000000, -0.000000000000000000, -1.000000000000000000 ) ) ;
#12199 = PLANE ( 'NONE',  #16009 ) ;
#12200 = DIRECTION ( 'NONE',  ( -0.000000000000000000, -0.000000000000000000, -1.000000000000000000 ) ) ;
#12201 = CARTESIAN_POINT ( 'NONE',  ( -107.3221550338875687, 22.24192588826928585, 83.00000000000001421 ) ) ;
#12202 = CIRCLE ( 'NONE', #5758, 14.13483123440684253 ) ;
#12203 = DIRECTION ( 'NONE',  ( -0.000000000000000000, -0.000000000000000000, 1.000000000000000000 ) ) ;
#12204 = DIRECTION ( 'NONE',  ( -0.000000000000000000, -1.000000000000000000, -0.000000000000000000 ) ) ;
#12205 = DIRECTION ( 'NONE',  ( -0.000000000000000000, -0.000000000000000000, 1.000000000000000000 ) ) ;
#12206 = VECTOR ( 'NONE', #23346, 1000.000000000000000 ) ;
#12207 = DIRECTION ( 'NONE',  ( 0.000000000000000000, 0.000000000000000000, -1.000000000000000000 ) ) ;
#12208 = VECTOR ( 'NONE', #20989, 1000.000000000000000 ) ;
#12209 = ORIENTED_EDGE ( 'NONE', *, *, #18754, .T. ) ;
#12210 = EDGE_CURVE ( 'NONE', #17211, #1493, #919, .T. ) ;
#12211 = EDGE_CURVE ( 'NONE', #88, #17838, #12107, .T. ) ;
#12212 = LINE ( 'NONE', #23389, #11914 ) ;
#12213 = CARTESIAN_POINT ( 'NONE',  ( 109.6721745451464045, 96.60743919220468001, -100.0000000000000142 ) ) ;
#12214 = DIRECTION ( 'NONE',  ( 0.8916010070293383105, -0.4528218681383106015, 0.000000000000000000 ) ) ;
#12215 = AXIS2_PLACEMENT_3D ( 'NONE', #21757, #8961, #4636 ) ;
#12217 = VERTEX_POINT ( 'NONE', #23035 ) ;
#12216 = ORIENTED_EDGE ( 'NONE', *, *, #15762, .T. ) ;
#12218 = DIRECTION ( 'NONE',  ( 0.05364526231779760679, -0.9985600561963485777, 0.000000000000000000 ) ) ;
#12219 = VERTEX_POINT ( 'NONE', #3489 ) ;
#12220 = ORIENTED_EDGE ( 'NONE', *, *, #21007, .T. ) ;
#12221 = VERTEX_POINT ( 'NONE', #14147 ) ;
#12222 = ORIENTED_EDGE ( 'NONE', *, *, #25990, .F. ) ;
#12223 = VECTOR ( 'NONE', #845, 1000.000000000000114 ) ;
#12224 = ORIENTED_EDGE ( 'NONE', *, *, #13256, .F. ) ;
#12225 = ORIENTED_EDGE ( 'NONE', *, *, #15008, .F. ) ;
#12227 = EDGE_CURVE ( 'NONE', #22223, #23150, #10727, .T. ) ;
#12226 = VECTOR ( 'NONE', #16903, 1000.000000000000000 ) ;
#12228 = DIRECTION ( 'NONE',  ( 0.000000000000000000, -1.000000000000000000, 0.000000000000000000 ) ) ;
#12229 = EDGE_CURVE ( 'NONE', #5272, #9114, #20879, .T. ) ;
#12230 = CARTESIAN_POINT ( 'NONE',  ( 157.4999999999998579, 93.35231212089433939, 45.00000000000000000 ) ) ;
#12231 = EDGE_CURVE ( 'NONE', #12519, #506, #27200, .T. ) ;
#12232 = VECTOR ( 'NONE', #9955, 1000.000000000000114 ) ;
#12233 = CARTESIAN_POINT ( 'NONE',  ( 122.8247714198256944, 204.1329331941749672, 45.00000000000000000 ) ) ;
#12234 = CARTESIAN_POINT ( 'NONE',  ( 157.4999999999998579, 196.1751874286831026, 45.00000000000000000 ) ) ;
#12235 = CARTESIAN_POINT ( 'NONE',  ( 79.99999999999991473, 140.0000000000000000, -15.00000000000000000 ) ) ;
#12236 = CARTESIAN_POINT ( 'NONE',  ( 0.000000000000000000, 330.0000000000000000, 100.0000000000000142 ) ) ;
#12237 = CARTESIAN_POINT ( 'NONE',  ( -222.0767938393173893, 71.52268347900216838, -20.18230367956038407 ) ) ;
#12238 = LINE ( 'NONE', #10345, #2209 ) ;
#12239 = SPHERICAL_SURFACE ( 'NONE', #12804, 30.00000000000000000 ) ;
#12240 = CARTESIAN_POINT ( 'NONE',  ( -68.57415822541635464, 80.97823757117562593, 80.00000000000001421 ) ) ;
#12241 = ORIENTED_EDGE ( 'NONE', *, *, #17710, .T. ) ;
#12242 = AXIS2_PLACEMENT_3D ( 'NONE', #27724, #8065, #7921 ) ;
#12243 = CARTESIAN_POINT ( 'NONE',  ( -195.0176442371520693, 99.46973748894193079, 32.52229805665887596 ) ) ;
#12244 = DIRECTION ( 'NONE',  ( -0.2066290158914539099, 0.9784193629480814058, 0.000000000000000000 ) ) ;
#12245 = EDGE_LOOP ( 'NONE', ( #11936, #10013 ) ) ;
#12246 = CARTESIAN_POINT ( 'NONE',  ( 0.000000000000000000, 0.000000000000000000, 0.000000000000000000 ) ) ;
#12247 = AXIS2_PLACEMENT_3D ( 'NONE', #6103, #3943, #12308 ) ;
#12248 = ORIENTED_EDGE ( 'NONE', *, *, #20192, .T. ) ;
#12249 = ORIENTED_EDGE ( 'NONE', *, *, #1654, .T. ) ;
#12250 = CARTESIAN_POINT ( 'NONE',  ( 106.3487426207432804, 91.82653269718771583, 100.0000000000000142 ) ) ;
#12251 = LINE ( 'NONE', #25575, #24595 ) ;
#12252 = ORIENTED_EDGE ( 'NONE', *, *, #9191, .T. ) ;
#12253 = ADVANCED_FACE ( 'NONE', ( #3203 ), #9964, .F. ) ;
#12254 = ORIENTED_EDGE ( 'NONE', *, *, #16876, .T. ) ;
#12255 = CARTESIAN_POINT ( 'NONE',  ( 90.17595424773269031, 111.7661400908363731, -72.22656249986501109 ) ) ;
#12256 = EDGE_CURVE ( 'NONE', #6469, #24347, #25328, .T. ) ;
#12257 = CARTESIAN_POINT ( 'NONE',  ( 94.28021150171387887, 231.3879905774517454, 18.61204911420563590 ) ) ;
#12258 = EDGE_CURVE ( 'NONE', #7010, #27514, #13870, .T. ) ;
#12259 = DIRECTION ( 'NONE',  ( 1.000000000000000000, -1.387778780781444413E-14, 0.000000000000000000 ) ) ;
#12260 = VERTEX_POINT ( 'NONE', #18584 ) ;
#12261 = CARTESIAN_POINT ( 'NONE',  ( 100.8904249506254018, 86.57652225510716448, 100.0000000000000142 ) ) ;
#12262 = VERTEX_POINT ( 'NONE', #27332 ) ;
#12263 = TOROIDAL_SURFACE ( 'NONE', #22341, 21.49999999999998224, 1.000000000000000000 ) ;
#12264 = FACE_OUTER_BOUND ( 'NONE', #19083, .T. ) ;
#12265 = DIRECTION ( 'NONE',  ( 1.000000000000000000, 0.000000000000000000, 0.000000000000000000 ) ) ;
#12266 = DIRECTION ( 'NONE',  ( 0.8916010070293584056, -0.4528218681382712996, 0.000000000000000000 ) ) ;
#12267 = CARTESIAN_POINT ( 'NONE',  ( 150.8670668058245212, 232.1752285801742630, -45.00000000000000000 ) ) ;
#12268 = FACE_OUTER_BOUND ( 'NONE', #14603, .T. ) ;
#12269 = CARTESIAN_POINT ( 'NONE',  ( 157.4999999999997158, 258.8720626163585621, 45.00000000000000000 ) ) ;
#12270 = CARTESIAN_POINT ( 'NONE',  ( 163.0755097476689741, 209.4274900230976471, -148.4939404368777787 ) ) ;
#12271 = ORIENTED_EDGE ( 'NONE', *, *, #11101, .T. ) ;
#12272 = DIRECTION ( 'NONE',  ( -0.8916010070295011802, -0.4528218681379903021, 0.000000000000000000 ) ) ;
#12273 = DIRECTION ( 'NONE',  ( 1.000000000000000000, 0.000000000000000000, 0.000000000000000000 ) ) ;
#12274 = PLANE ( 'NONE',  #23945 ) ;
#12275 = CARTESIAN_POINT ( 'NONE',  ( -221.3650667873343139, -91.18033988749901653, 0.000000000000000000 ) ) ;
#12276 = ORIENTED_EDGE ( 'NONE', *, *, #9034, .T. ) ;
#12277 = CARTESIAN_POINT ( 'NONE',  ( 157.4999999999998579, 191.1594374136689964, -45.00000000000000000 ) ) ;
#12278 = EDGE_LOOP ( 'NONE', ( #5757, #7008, #6295, #8867 ) ) ;
#12279 = DIRECTION ( 'NONE',  ( 1.530283246943720875E-16, -1.000000000000000000, 0.000000000000000000 ) ) ;
#12280 = DIRECTION ( 'NONE',  ( -3.053113317719176147E-15, -4.035281788239917819E-31, -1.000000000000000000 ) ) ;
#12281 = CARTESIAN_POINT ( 'NONE',  ( -221.3650667873343139, -91.18033988749901653, 0.000000000000000000 ) ) ;
#12282 = EDGE_LOOP ( 'NONE', ( #1771, #21818, #17669, #12648 ) ) ;
#12283 = PLANE ( 'NONE',  #27572 ) ;
#12284 = DIRECTION ( 'NONE',  ( -0.000000000000000000, 0.000000000000000000, -1.000000000000000000 ) ) ;
#12285 = VERTEX_POINT ( 'NONE', #7671 ) ;
#12286 = CIRCLE ( 'NONE', #19606, 6.000000000000005329 ) ;
#12287 = VECTOR ( 'NONE', #16078, 1000.000000000000000 ) ;
#12288 = EDGE_CURVE ( 'NONE', #27871, #11282, #25186, .T. ) ;
#12289 = DIRECTION ( 'NONE',  ( 0.4528218681378310406, -0.8916010070295820045, 0.000000000000000000 ) ) ;
#12290 = DIRECTION ( 'NONE',  ( 0.4528218681370124177, 0.8916010070299977830, -0.000000000000000000 ) ) ;
#12291 = VERTEX_POINT ( 'NONE', #18861 ) ;
#12292 = ORIENTED_EDGE ( 'NONE', *, *, #9537, .T. ) ;
#12293 = EDGE_CURVE ( 'NONE', #17838, #17982, #16716, .T. ) ;
#12294 = DIRECTION ( 'NONE',  ( 0.4999999999999985012, 0.8660254037844394848, 0.000000000000000000 ) ) ;
#12295 = ORIENTED_EDGE ( 'NONE', *, *, #26454, .T. ) ;
#12296 = EDGE_CURVE ( 'NONE', #16250, #11334, #2931, .T. ) ;
#12297 = ORIENTED_EDGE ( 'NONE', *, *, #19617, .T. ) ;
#12298 = ORIENTED_EDGE ( 'NONE', *, *, #8149, .F. ) ;
#12299 = PLANE ( 'NONE',  #15754 ) ;
#12300 = AXIS2_PLACEMENT_3D ( 'NONE', #23592, #10521, #19279 ) ;
#12301 = PRODUCT_RELATED_PRODUCT_CATEGORY ( 'part', '', ( #4537 ) ) ;
#12302 = CARTESIAN_POINT ( 'NONE',  ( -226.9194690495523332, 131.5555540326517985, 13.00000000000000000 ) ) ;
#12303 = DIRECTION ( 'NONE',  ( 1.000000000000000000, -0.000000000000000000, -0.000000000000000000 ) ) ;
#12304 = VECTOR ( 'NONE', #123, 1000.000000000000114 ) ;
#12305 = CARTESIAN_POINT ( 'NONE',  ( 158.0000000000008242, 126.2086247222394206, 45.00000000000000000 ) ) ;
#12306 = LINE ( 'NONE', #16746, #25939 ) ;
#12307 = DIRECTION ( 'NONE',  ( 1.321694076934710155E-16, -1.000000000000000000, 0.000000000000000000 ) ) ;
#12308 = DIRECTION ( 'NONE',  ( -0.000000000000000000, 0.000000000000000000, -1.000000000000000000 ) ) ;
#12309 = LINE ( 'NONE', #23635, #13387 ) ;
#12310 = CARTESIAN_POINT ( 'NONE',  ( 157.4999999999995737, 203.6988124512014338, -45.00000000000000000 ) ) ;
#12311 = DIRECTION ( 'NONE',  ( 1.321694076934710155E-16, -1.000000000000000000, 0.000000000000000000 ) ) ;
#12312 = ORIENTED_EDGE ( 'NONE', *, *, #21657, .T. ) ;
#12313 = DIRECTION ( 'NONE',  ( 0.8916010070296124246, -0.4528218681377710886, 0.000000000000000000 ) ) ;
#12314 = CARTESIAN_POINT ( 'NONE',  ( 94.61298883701873308, 240.5205049088891371, -8.728139299124077155 ) ) ;
#12315 = DIRECTION ( 'NONE',  ( -0.000000000000000000, -0.000000000000000000, -1.000000000000000000 ) ) ;
#12316 = DIRECTION ( 'NONE',  ( 0.000000000000000000, 0.000000000000000000, -1.000000000000000000 ) ) ;
#12317 = CARTESIAN_POINT ( 'NONE',  ( -277.2150368962633706, -170.0000000000001137, -110.0000000000000284 ) ) ;
#12318 = EDGE_CURVE ( 'NONE', #11476, #26259, #5790, .T. ) ;
#12319 = ORIENTED_EDGE ( 'NONE', *, *, #23496, .F. ) ;
#12320 = AXIS2_PLACEMENT_3D ( 'NONE', #26987, #5154, #15661 ) ;
#12321 = EDGE_CURVE ( 'NONE', #23236, #11585, #6210, .T. ) ;
#12322 = CARTESIAN_POINT ( 'NONE',  ( 157.4999999999997158, 258.8720626163585621, 45.00000000000000000 ) ) ;
#12323 = ORIENTED_EDGE ( 'NONE', *, *, #14096, .T. ) ;
#12324 = FACE_OUTER_BOUND ( 'NONE', #21236, .T. ) ;
#12325 = CIRCLE ( 'NONE', #1730, 22.49999999999999289 ) ;
#12326 = ORIENTED_EDGE ( 'NONE', *, *, #22561, .T. ) ;
#12327 = VERTEX_POINT ( 'NONE', #21729 ) ;
#12328 = CARTESIAN_POINT ( 'NONE',  ( -97.91344426061895945, 136.1593943688571926, 15.19680741217146824 ) ) ;
#12329 = EDGE_CURVE ( 'NONE', #14397, #27215, #6069, .T. ) ;
#12330 = ORIENTED_EDGE ( 'NONE', *, *, #142, .F. ) ;
#12331 = VERTEX_POINT ( 'NONE', #12980 ) ;
#12332 = CARTESIAN_POINT ( 'NONE',  ( 134.9999999999998579, 468.7804619981748147, -145.0000000000000000 ) ) ;
#12333 = SPHERICAL_SURFACE ( 'NONE', #9143, 30.00000000000000000 ) ;
#12334 = DIRECTION ( 'NONE',  ( 0.8916010070298556744, -0.4528218681372921384, 0.000000000000000000 ) ) ;
#12335 = EDGE_CURVE ( 'NONE', #2081, #17634, #14853, .T. ) ;
#12336 = CARTESIAN_POINT ( 'NONE',  ( 157.4999999999998579, 123.4468122109788482, 45.00000000000000000 ) ) ;
#12337 = CARTESIAN_POINT ( 'NONE',  ( -275.9795250186070916, -170.0000000000001137, -91.22351627327833512 ) ) ;
#12339 = LINE ( 'NONE', #1399, #27435 ) ;
#12338 = VECTOR ( 'NONE', #5117, 1000.000000000000000 ) ;
#12340 = CARTESIAN_POINT ( 'NONE',  ( -266.9750954100557010, -170.7663605388744941, 89.20968119495026372 ) ) ;
#12341 = CARTESIAN_POINT ( 'NONE',  ( 367.9108539694884144, 44.41075299063184190, 74.99887465166234790 ) ) ;
#12342 = AXIS2_PLACEMENT_3D ( 'NONE', #18513, #7597, #3546 ) ;
#12343 = DIRECTION ( 'NONE',  ( -0.8916010070293383105, -0.4528218681383106015, 0.000000000000000000 ) ) ;
#12344 = DIRECTION ( 'NONE',  ( 0.000000000000000000, -1.000000000000000000, 0.000000000000000000 ) ) ;
#12345 = DIRECTION ( 'NONE',  ( 0.000000000000000000, -1.000000000000000000, 0.000000000000000000 ) ) ;
#12346 = ORIENTED_EDGE ( 'NONE', *, *, #20942, .F. ) ;
#12347 = ADVANCED_FACE ( 'NONE', ( #10386 ), #1476, .F. ) ;
#12348 = CARTESIAN_POINT ( 'NONE',  ( -42.54774212103357200, -18.98692024693243852, 99.90775213666447030 ) ) ;
#12349 = LINE ( 'NONE', #16512, #5569 ) ;
#12351 = ORIENTED_EDGE ( 'NONE', *, *, #17845, .F. ) ;
#12350 = EDGE_LOOP ( 'NONE', ( #15995, #9137, #23608, #26395 ) ) ;
#12352 = EDGE_CURVE ( 'NONE', #10435, #2939, #21298, .T. ) ;
#12353 = CIRCLE ( 'NONE', #16910, 10.00000000000000888 ) ;
#12354 = DIRECTION ( 'NONE',  ( 1.000000000000000000, 0.000000000000000000, -0.000000000000000000 ) ) ;
#12355 = ORIENTED_EDGE ( 'NONE', *, *, #4980, .T. ) ;
#12356 = VERTEX_POINT ( 'NONE', #14990 ) ;
#12357 = ORIENTED_EDGE ( 'NONE', *, *, #8991, .F. ) ;
#12358 = CIRCLE ( 'NONE', #13737, 24.07986109634097005 ) ;
#12359 = AXIS2_PLACEMENT_3D ( 'NONE', #14805, #21398, #1711 ) ;
#12360 = VERTEX_POINT ( 'NONE', #3768 ) ;
#12361 = ORIENTED_EDGE ( 'NONE', *, *, #8470, .T. ) ;
#12362 = ORIENTED_EDGE ( 'NONE', *, *, #19827, .T. ) ;
#12363 = VECTOR ( 'NONE', #17296, 999.9999999999998863 ) ;
#12364 = DIRECTION ( 'NONE',  ( -1.000000000000000000, -2.602085213965211135E-16, -0.000000000000000000 ) ) ;
#12365 = VECTOR ( 'NONE', #1599, 1000.000000000000114 ) ;
#12366 = ADVANCED_FACE ( 'NONE', ( #3909 ), #25468, .F. ) ;
#12367 = ADVANCED_FACE ( 'NONE', ( #23317 ), #21156, .F. ) ;
#12368 = LINE ( 'NONE', #21106, #11003 ) ;
#12369 = LINE ( 'NONE', #21107, #24023 ) ;
#12370 = DIRECTION ( 'NONE',  ( 0.000000000000000000, -1.000000000000000000, 0.000000000000000000 ) ) ;
#12371 = VECTOR ( 'NONE', #12560, 1000.000000000000227 ) ;
#12372 = VECTOR ( 'NONE', #454, 1000.000000000000000 ) ;
#12373 = CARTESIAN_POINT ( 'NONE',  ( -266.4635733393146779, -165.8461665555755076, -109.6876586681348584 ) ) ;
#12374 = CARTESIAN_POINT ( 'NONE',  ( 158.0000000000002274, 183.8897498949014278, 45.00000000000000000 ) ) ;
#12375 = DIRECTION ( 'NONE',  ( 1.000000000000000000, -0.000000000000000000, -0.000000000000000000 ) ) ;
#12376 = EDGE_CURVE ( 'NONE', #5352, #61, #3624, .T. ) ;
#12377 = CIRCLE ( 'NONE', #28393, 5.000000000000000888 ) ;
#12378 = LINE ( 'NONE', #5885, #10963 ) ;
#12379 = CARTESIAN_POINT ( 'NONE',  ( -54.22951502486254327, 83.26691194124390449, 45.00000000000000000 ) ) ;
#12380 = CYLINDRICAL_SURFACE ( 'NONE', #2803, 6.000000000000032863 ) ;
#12381 = DIRECTION ( 'NONE',  ( 0.000000000000000000, 0.000000000000000000, -1.000000000000000000 ) ) ;
#12382 = EDGE_LOOP ( 'NONE', ( #1922, #778, #2797, #14870 ) ) ;
#12383 = CARTESIAN_POINT ( 'NONE',  ( 41.00000000000000000, 5.000000000000000000, 0.000000000000000000 ) ) ;
#12385 = EDGE_CURVE ( 'NONE', #1176, #1637, #1615, .T. ) ;
#12384 = VECTOR ( 'NONE', #6301, 1000.000000000000000 ) ;
#12386 = CARTESIAN_POINT ( 'NONE',  ( -277.6780266850147427, -169.9634972840153466, -106.7968975218380763 ) ) ;
#12387 = EDGE_LOOP ( 'NONE', ( #11732, #12577, #21885, #5524 ) ) ;
#12388 = CARTESIAN_POINT ( 'NONE',  ( 223.4999999999996305, 258.6181251126050711, 1.387778780781445676E-14 ) ) ;
#12389 = EDGE_CURVE ( 'NONE', #20612, #26679, #8090, .T. ) ;
#12390 = ORIENTED_EDGE ( 'NONE', *, *, #956, .T. ) ;
#12391 = ORIENTED_EDGE ( 'NONE', *, *, #10137, .F. ) ;
#12392 = CARTESIAN_POINT ( 'NONE',  ( 85.37729192592163940, 80.27798593822440409, 100.0000000000000142 ) ) ;
#12393 = VECTOR ( 'NONE', #7216, 1000.000000000000000 ) ;
#12394 = CARTESIAN_POINT ( 'NONE',  ( 65.00000000000000000, -120.0000000000000995, -75.99999999999998579 ) ) ;
#12395 = ORIENTED_EDGE ( 'NONE', *, *, #18802, .T. ) ;
#12396 = VERTEX_POINT ( 'NONE', #23884 ) ;
#12397 = CARTESIAN_POINT ( 'NONE',  ( 157.4999999999998010, 233.7933125412885147, 45.00000000000000000 ) ) ;
#12398 = AXIS2_PLACEMENT_3D ( 'NONE', #6574, #26102, #9015 ) ;
#12399 = CARTESIAN_POINT ( 'NONE',  ( 217.4999999999996305, 133.0668745871126930, -36.86484227207694886 ) ) ;
#12400 = DIRECTION ( 'NONE',  ( 0.4528218681378310406, -0.8916010070295820045, 0.000000000000000000 ) ) ;
#12401 = VERTEX_POINT ( 'NONE', #28029 ) ;
#12402 = CARTESIAN_POINT ( 'NONE',  ( 117.1152841538673073, 116.0550883417529207, 100.0000000000000142 ) ) ;
#12403 = ORIENTED_EDGE ( 'NONE', *, *, #11905, .F. ) ;
#12404 = DIRECTION ( 'NONE',  ( 1.000000000000000000, -0.000000000000000000, -0.000000000000000000 ) ) ;
#12405 = DIRECTION ( 'NONE',  ( 0.000000000000000000, 0.000000000000000000, 1.000000000000000000 ) ) ;
#12406 = DIRECTION ( 'NONE',  ( -0.9654425086906591735, 0.2448377981135679837, 0.08930405941493638200 ) ) ;
#12407 = DIRECTION ( 'NONE',  ( -0.000000000000000000, -0.000000000000000000, -1.000000000000000000 ) ) ;
#12408 = DIRECTION ( 'NONE',  ( -0.000000000000000000, -0.000000000000000000, -1.000000000000000000 ) ) ;
#12409 = DIRECTION ( 'NONE',  ( 0.6681556583950049033, -0.7440215159219103480, 0.000000000000000000 ) ) ;
#12410 = CARTESIAN_POINT ( 'NONE',  ( 161.8971595647778088, 206.7117171029577207, -150.6809294437986466 ) ) ;
#12411 = ORIENTED_EDGE ( 'NONE', *, *, #22501, .F. ) ;
#12412 = AXIS2_PLACEMENT_3D ( 'NONE', #525, #13900, #9575 ) ;
#12413 = DIRECTION ( 'NONE',  ( -1.000000000000000000, 0.000000000000000000, 0.000000000000000000 ) ) ;
#12414 = DIRECTION ( 'NONE',  ( 0.000000000000000000, 0.000000000000000000, 1.000000000000000000 ) ) ;
#12415 = LINE ( 'NONE', #6067, #1455 ) ;
#12416 = DIRECTION ( 'NONE',  ( 0.8916010070299977830, -0.4528218681370124177, 0.000000000000000000 ) ) ;
#12417 = EDGE_LOOP ( 'NONE', ( #15251, #20649, #15366, #23754 ) ) ;
#12418 = PLANE ( 'NONE',  #19695 ) ;
#12419 = EDGE_CURVE ( 'NONE', #7618, #22209, #14701, .T. ) ;
#12420 = AXIS2_PLACEMENT_3D ( 'NONE', #21533, #19667, #23841 ) ;
#12421 = VERTEX_POINT ( 'NONE', #28309 ) ;
#12422 = APPLICATION_CONTEXT ( 'automotive_design' ) ;
#12423 = CARTESIAN_POINT ( 'NONE',  ( -195.0245025301963722, 99.69673397905764034, 31.69035508706320670 ) ) ;
#12424 = CARTESIAN_POINT ( 'NONE',  ( 158.0000000000003695, 173.3503748573662051, -45.00000000000000000 ) ) ;
#12425 = LINE ( 'NONE', #5372, #10329 ) ;
#12426 = VERTEX_POINT ( 'NONE', #27889 ) ;
#12427 = DIRECTION ( 'NONE',  ( -0.8916010070296838119, -0.4528218681376305899, 0.000000000000000000 ) ) ;
#12428 = ORIENTED_EDGE ( 'NONE', *, *, #18408, .T. ) ;
#12429 = CARTESIAN_POINT ( 'NONE',  ( 157.4999999999998579, 125.9546872184859012, 45.00000000000000000 ) ) ;
#12430 = CARTESIAN_POINT ( 'NONE',  ( -210.0000000000000568, -220.0000000000000853, -110.0000000000000284 ) ) ;
#12431 = VERTEX_POINT ( 'NONE', #8657 ) ;
#12432 = ORIENTED_EDGE ( 'NONE', *, *, #3620, .F. ) ;
#12433 = DIRECTION ( 'NONE',  ( 1.000000000000000000, -0.000000000000000000, -0.000000000000000000 ) ) ;
#12434 = ORIENTED_EDGE ( 'NONE', *, *, #26038, .F. ) ;
#12435 = VECTOR ( 'NONE', #20726, 1000.000000000000000 ) ;
#12436 = EDGE_CURVE ( 'NONE', #24234, #16719, #8230, .T. ) ;
#12437 = ORIENTED_EDGE ( 'NONE', *, *, #13405, .T. ) ;
#12438 = EDGE_LOOP ( 'NONE', ( #13509, #22096, #14724, #16653 ) ) ;
#12439 = DIRECTION ( 'NONE',  ( 0.000000000000000000, 0.000000000000000000, -1.000000000000000000 ) ) ;
#12440 = VECTOR ( 'NONE', #3487, 1000.000000000000000 ) ;
#12441 = ADVANCED_FACE ( 'NONE', ( #17133 ), #25889, .F. ) ;
#12442 = CARTESIAN_POINT ( 'NONE',  ( 187.4999999999996305, 288.9665627064425166, -45.00000000000000000 ) ) ;
#12443 = CARTESIAN_POINT ( 'NONE',  ( 145.9999999999998863, 220.0000000000000284, -100.0000000000000142 ) ) ;
#12444 = CARTESIAN_POINT ( 'NONE',  ( -225.7036482868739427, -91.18033988749901653, 0.000000000000000000 ) ) ;
#12445 = DIRECTION ( 'NONE',  ( 1.000000000000000000, -0.000000000000000000, -0.000000000000000000 ) ) ;
#12446 = CARTESIAN_POINT ( 'NONE',  ( -220.9458266506740927, 71.36862438102546946, -20.99673689147822486 ) ) ;
#12447 = DIRECTION ( 'NONE',  ( -0.9586565047779720405, -0.2845658198851049314, -0.000000000000000000 ) ) ;
#12448 = EDGE_CURVE ( 'NONE', #6469, #19409, #10669, .T. ) ;
#12449 = DIRECTION ( 'NONE',  ( 0.000000000000000000, -1.000000000000000000, 0.000000000000000000 ) ) ;
#12450 = CARTESIAN_POINT ( 'NONE',  ( 0.000000000000000000, -1.249999999999999112, -6.997769477110050929 ) ) ;
#12451 = CARTESIAN_POINT ( 'NONE',  ( 158.0000000000000853, 198.4291249324366504, 45.00000000000000000 ) ) ;
#12452 = VERTEX_POINT ( 'NONE', #13123 ) ;
#12453 = ADVANCED_FACE ( 'NONE', ( #22147 ), #22003, .F. ) ;
#12454 = DIRECTION ( 'NONE',  ( 1.000000000000000000, -0.000000000000000000, -0.000000000000000000 ) ) ;
#12455 = EDGE_CURVE ( 'NONE', #17982, #7779, #17549, .T. ) ;
#12456 = CARTESIAN_POINT ( 'NONE',  ( 117.5127944162877753, 203.5381304684075019, 45.00000000000000000 ) ) ;
#12457 = DIRECTION ( 'NONE',  ( 0.8916010070296632728, -0.4528218681376712240, 0.000000000000000000 ) ) ;
#12458 = DIRECTION ( 'NONE',  ( 0.000000000000000000, -1.000000000000000000, 0.000000000000000000 ) ) ;
#12459 = LINE ( 'NONE', #12317, #21646 ) ;
#12460 = ORIENTED_EDGE ( 'NONE', *, *, #12963, .F. ) ;
#12461 = VECTOR ( 'NONE', #13831, 1000.000000000000114 ) ;
#12462 = DIRECTION ( 'NONE',  ( 0.4999999999999920064, -0.8660254037844432595, 0.000000000000000000 ) ) ;
#12463 = ORIENTED_EDGE ( 'NONE', *, *, #15147, .T. ) ;
#12464 = CARTESIAN_POINT ( 'NONE',  ( 144.9999999999998863, 220.0000000000000284, 45.00000000000000000 ) ) ;
#12465 = EDGE_LOOP ( 'NONE', ( #14679, #4462, #13228, #13734 ) ) ;
#12466 = EDGE_LOOP ( 'NONE', ( #5022, #19923, #10259, #19513 ) ) ;
#12467 = CARTESIAN_POINT ( 'NONE',  ( -86.54597169974458382, 136.4599361015214072, 15.16231345941510433 ) ) ;
#12468 = VERTEX_POINT ( 'NONE', #21867 ) ;
#12469 = ORIENTED_EDGE ( 'NONE', *, *, #6660, .F. ) ;
#12470 = CARTESIAN_POINT ( 'NONE',  ( 112.8464227643159035, 224.0613302109408380, 96.99047740776141779 ) ) ;
#12471 = CARTESIAN_POINT ( 'NONE',  ( 158.0000000000001421, 193.4133749174225443, -45.00000000000000000 ) ) ;
#12472 = CARTESIAN_POINT ( 'NONE',  ( -260.0000000000001137, -220.0000000000000853, 60.00000000000002132 ) ) ;
#12473 = VECTOR ( 'NONE', #2524, 1000.000000000000000 ) ;
#12474 = CARTESIAN_POINT ( 'NONE',  ( 158.0000000000003411, 175.8582498648732440, 45.00000000000000000 ) ) ;
#12475 = VECTOR ( 'NONE', #2940, 1000.000000000000000 ) ;
#12476 = EDGE_CURVE ( 'NONE', #2290, #2012, #13053, .T. ) ;
#12477 = AXIS2_PLACEMENT_3D ( 'NONE', #17345, #19360, #8454 ) ;
#12478 = CARTESIAN_POINT ( 'NONE',  ( -267.5881315349600982, -170.6799793700724877, -89.03726891381465691 ) ) ;
#12479 = DIRECTION ( 'NONE',  ( -0.2066290158914389774, 0.9784193629480844034, 0.000000000000000000 ) ) ;
#12480 = EDGE_CURVE ( 'NONE', #27327, #21761, #8791, .T. ) ;
#12481 = DIRECTION ( 'NONE',  ( 1.000000000000000000, 0.000000000000000000, 0.000000000000000000 ) ) ;
#12482 = CARTESIAN_POINT ( 'NONE',  ( -221.2010484699854089, 88.15128852653619163, -15.79399925067323451 ) ) ;
#12483 = CARTESIAN_POINT ( 'NONE',  ( 132.3338888694437401, 249.8834866143649833, -150.3892986974657617 ) ) ;
#12484 = CARTESIAN_POINT ( 'NONE',  ( -224.8943620750042669, 87.10469160093204266, 16.59178732851365012 ) ) ;
#12485 = PLANE ( 'NONE',  #11084 ) ;
#12486 = FACE_OUTER_BOUND ( 'NONE', #7579, .T. ) ;
#12487 = LINE ( 'NONE', #14632, #4697 ) ;
#12488 = ORIENTED_EDGE ( 'NONE', *, *, #27421, .F. ) ;
#12489 = EDGE_CURVE ( 'NONE', #17959, #4884, #6638, .T. ) ;
#12490 = DIRECTION ( 'NONE',  ( -0.6533458216954761699, 0.7570595995514904919, 0.000000000000000000 ) ) ;
#12491 = DIRECTION ( 'NONE',  ( -1.000000000000000000, 0.000000000000000000, 0.000000000000000000 ) ) ;
#12493 = VERTEX_POINT ( 'NONE', #17411 ) ;
#12492 = ORIENTED_EDGE ( 'NONE', *, *, #19561, .F. ) ;
#12494 = CARTESIAN_POINT ( 'NONE',  ( 100.8286702512460664, 242.7181571222803882, -23.14229345413746231 ) ) ;
#12495 = VERTEX_POINT ( 'NONE', #17695 ) ;
#12496 = ORIENTED_EDGE ( 'NONE', *, *, #22723, .F. ) ;
#12497 = VECTOR ( 'NONE', #5664, 1000.000000000000000 ) ;
#12498 = EDGE_LOOP ( 'NONE', ( #2465, #24607, #27967, #14361 ) ) ;
#12499 = VECTOR ( 'NONE', #10290, 1000.000000000000000 ) ;
#12500 = EDGE_LOOP ( 'NONE', ( #16267, #28318, #22125, #13658 ) ) ;
#12501 = ORIENTED_EDGE ( 'NONE', *, *, #12385, .T. ) ;
#12502 = ORIENTED_EDGE ( 'NONE', *, *, #21182, .T. ) ;
#12503 = CARTESIAN_POINT ( 'NONE',  ( 118.0294372515228787, 204.4436508138956015, 45.00000000000000000 ) ) ;
#12504 = DIRECTION ( 'NONE',  ( -1.000000000000000000, 0.000000000000000000, 0.000000000000000000 ) ) ;
#12505 = CARTESIAN_POINT ( 'NONE',  ( 109.5123651676572933, 253.5802735191045656, -39.43351859324057784 ) ) ;
#12506 = VECTOR ( 'NONE', #25449, 1000.000000000000000 ) ;
#12507 = DIRECTION ( 'NONE',  ( 3.469446951953614189E-16, -1.000000000000000000, 0.000000000000000000 ) ) ;
#12508 = EDGE_CURVE ( 'NONE', #22333, #7588, #2175, .T. ) ;
#12509 = VECTOR ( 'NONE', #21546, 1000.000000000000114 ) ;
#12510 = CARTESIAN_POINT ( 'NONE',  ( 142.6536686473015152, 238.4775906502254941, 45.00000000000000000 ) ) ;
#12511 = FACE_BOUND ( 'NONE', #12636, .T. ) ;
#12512 = LINE ( 'NONE', #12790, #16095 ) ;
#12513 = CARTESIAN_POINT ( 'NONE',  ( -209.1631124584775705, 74.45386818103241922, -36.43774469185622422 ) ) ;
#12514 = VECTOR ( 'NONE', #1415, 1000.000000000000000 ) ;
#12515 = CARTESIAN_POINT ( 'NONE',  ( 111.7303663796180473, 201.0648462552355795, -148.6534330424975963 ) ) ;
#12516 = DIRECTION ( 'NONE',  ( -0.000000000000000000, -0.000000000000000000, 1.000000000000000000 ) ) ;
#12517 = CARTESIAN_POINT ( 'NONE',  ( 158.0000000000014495, 68.01962454207041731, 45.00000000000000000 ) ) ;
#12518 = DIRECTION ( 'NONE',  ( 0.8916010070299064116, -0.4528218681371922183, 0.000000000000000000 ) ) ;
#12519 = VERTEX_POINT ( 'NONE', #13543 ) ;
#12520 = CARTESIAN_POINT ( 'NONE',  ( -192.4212042216159944, 101.6389693173133253, 32.42120117541568192 ) ) ;
#12521 = EDGE_CURVE ( 'NONE', #24989, #3649, #2746, .T. ) ;
#12522 = EDGE_CURVE ( 'NONE', #21564, #26706, #24303, .T. ) ;
#12523 = CARTESIAN_POINT ( 'NONE',  ( 134.9999999999998579, 220.0000000000000284, 99.00000000000001421 ) ) ;
#12524 = ORIENTED_EDGE ( 'NONE', *, *, #5858, .T. ) ;
#12525 = CONTEXT_DEPENDENT_SHAPE_REPRESENTATION ( #16276, #23810 ) ;
#12526 = VERTEX_POINT ( 'NONE', #11093 ) ;
#12527 = AXIS2_PLACEMENT_3D ( 'NONE', #12472, #3969, #10588 ) ;
#12528 = ORIENTED_EDGE ( 'NONE', *, *, #7031, .T. ) ;
#12529 = TOROIDAL_SURFACE ( 'NONE', #22617, 19.29759039828519818, 4.355764593064427537 ) ;
#12530 = CARTESIAN_POINT ( 'NONE',  ( 79.99999999999991473, 80.00000000000001421, 100.0000000000000142 ) ) ;
#12531 = DIRECTION ( 'NONE',  ( -0.000000000000000000, -0.000000000000000000, -1.000000000000000000 ) ) ;
#12532 = ORIENTED_EDGE ( 'NONE', *, *, #24973, .T. ) ;
#12533 = VECTOR ( 'NONE', #25989, 1000.000000000000000 ) ;
#12535 = EDGE_CURVE ( 'NONE', #15146, #2640, #16265, .T. ) ;
#12534 = ORIENTED_EDGE ( 'NONE', *, *, #22789, .F. ) ;
#12536 = DIRECTION ( 'NONE',  ( -0.8916010070293584056, 0.4528218681382713551, 0.000000000000000000 ) ) ;
#12537 = VECTOR ( 'NONE', #12883, 1000.000000000000000 ) ;
#12538 = ADVANCED_FACE ( 'NONE', ( #13398 ), #10952, .T. ) ;
#12539 = CARTESIAN_POINT ( 'NONE',  ( 158.0000000000014779, 63.51174953456337136, 45.00000000000000000 ) ) ;
#12540 = CARTESIAN_POINT ( 'NONE',  ( -160.8326600028555902, 120.2355194873575073, -21.37420696376537776 ) ) ;
#12541 = ORIENTED_EDGE ( 'NONE', *, *, #14579, .T. ) ;
#12542 = DIRECTION ( 'NONE',  ( 1.000000000000000000, 0.000000000000000000, -2.064684994405763843E-16 ) ) ;
#12543 = EDGE_LOOP ( 'NONE', ( #17147, #14335, #3925, #25683 ) ) ;
#12544 = CARTESIAN_POINT ( 'NONE',  ( -160.0000000000000284, 59.99999999999994316, 100.0000000000000142 ) ) ;
#12545 = EDGE_CURVE ( 'NONE', #27805, #6438, #24031, .T. ) ;
#12546 = PLANE ( 'NONE',  #27708 ) ;
#12547 = DIRECTION ( 'NONE',  ( 1.000000000000000000, 0.000000000000000000, -0.000000000000000000 ) ) ;
#12548 = FACE_OUTER_BOUND ( 'NONE', #15787, .T. ) ;
#12549 = VECTOR ( 'NONE', #6233, 1000.000000000000000 ) ;
#12550 = PLANE ( 'NONE',  #21597 ) ;
#12551 = CARTESIAN_POINT ( 'NONE',  ( -187.2855578089503013, 105.0618758895388254, -32.61441565267596587 ) ) ;
#12552 = ORIENTED_EDGE ( 'NONE', *, *, #17975, .F. ) ;
#12553 = AXIS2_PLACEMENT_3D ( 'NONE', #7107, #19890, #2644 ) ;
#12554 = LINE ( 'NONE', #14848, #16898 ) ;
#12555 = DIRECTION ( 'NONE',  ( 0.000000000000000000, 0.000000000000000000, 1.000000000000000000 ) ) ;
#12556 = FACE_OUTER_BOUND ( 'NONE', #26493, .T. ) ;
#12557 = AXIS2_PLACEMENT_3D ( 'NONE', #19641, #17338, #23529 ) ;
#12558 = DIRECTION ( 'NONE',  ( -0.000000000000000000, -0.000000000000000000, -1.000000000000000000 ) ) ;
#12559 = VERTEX_POINT ( 'NONE', #4466 ) ;
#12560 = DIRECTION ( 'NONE',  ( 0.8916010070294699830, -0.4528218681380514199, 0.000000000000000000 ) ) ;
#12561 = EDGE_CURVE ( 'NONE', #20475, #10473, #11387, .T. ) ;
#12562 = DIRECTION ( 'NONE',  ( 0.000000000000000000, 0.000000000000000000, -1.000000000000000000 ) ) ;
#12563 = CARTESIAN_POINT ( 'NONE',  ( -31.71380104971701641, 128.0308663543026739, -17.49104459963816893 ) ) ;
#12564 = CARTESIAN_POINT ( 'NONE',  ( -215.9344744818343429, 87.83801675608414428, 18.87891717999596253 ) ) ;
#12565 = EDGE_LOOP ( 'NONE', ( #18875, #3078, #3780, #26515 ) ) ;
#12566 = CARTESIAN_POINT ( 'NONE',  ( -236.8177751472017007, 82.33896643611701904, 15.00000000000000000 ) ) ;
#12567 = ORIENTED_EDGE ( 'NONE', *, *, #6434, .T. ) ;
#12568 = LINE ( 'NONE', #10683, #15690 ) ;
#12569 = CARTESIAN_POINT ( 'NONE',  ( 109.9895023066273723, 259.3387059742136671, 43.85457132728548402 ) ) ;
#12570 = ORIENTED_EDGE ( 'NONE', *, *, #12335, .T. ) ;
#12571 = AXIS2_PLACEMENT_3D ( 'NONE', #21679, #1992, #2409 ) ;
#12572 = ORIENTED_EDGE ( 'NONE', *, *, #1722, .F. ) ;
#12573 = DIRECTION ( 'NONE',  ( -0.000000000000000000, -0.3247168404252948060, -0.9458112779747414045 ) ) ;
#12574 = ORIENTED_EDGE ( 'NONE', *, *, #3638, .T. ) ;
#12575 = AXIS2_PLACEMENT_3D ( 'NONE', #22312, #8808, #22022 ) ;
#12576 = PRODUCT ( 'High-Force Electromagnet Base Block', 'High-Force Electromagnet Base Block', '', ( #10926 ) ) ;
#12577 = ORIENTED_EDGE ( 'NONE', *, *, #21100, .F. ) ;
#12578 = ORIENTED_EDGE ( 'NONE', *, *, #19957, .F. ) ;
#12579 = VECTOR ( 'NONE', #1787, 1000.000000000000114 ) ;
#12580 = EDGE_CURVE ( 'NONE', #18325, #6225, #24593, .T. ) ;
#12581 = DIRECTION ( 'NONE',  ( -0.8916010070296834789, -0.4528218681376312005, 0.000000000000000000 ) ) ;
#12582 = ADVANCED_FACE ( 'NONE', ( #15553 ), #9223, .F. ) ;
#12583 = FACE_OUTER_BOUND ( 'NONE', #5101, .T. ) ;
#12584 = EDGE_CURVE ( 'NONE', #9066, #22237, #15698, .T. ) ;
#12585 = CARTESIAN_POINT ( 'NONE',  ( 158.0000000000017053, 43.44874947450702507, -45.00000000000000000 ) ) ;
#12586 = CARTESIAN_POINT ( 'NONE',  ( 6.071532165918828775E-15, -70.00000000000002842, -70.00000000000001421 ) ) ;
#12587 = DIRECTION ( 'NONE',  ( 0.000000000000000000, -1.000000000000000000, 0.000000000000000000 ) ) ;
#12588 = LINE ( 'NONE', #1778, #3910 ) ;
#12589 = CARTESIAN_POINT ( 'NONE',  ( -235.8599852676175601, 67.86969485657397172, -15.13802962878465763 ) ) ;
#12590 = EDGE_LOOP ( 'NONE', ( #8098, #14969, #25763, #25932 ) ) ;
#12591 = LINE ( 'NONE', #14884, #5787 ) ;
#12592 = DIRECTION ( 'NONE',  ( 0.7440215159218956931, -0.6681556583950213346, 0.000000000000000000 ) ) ;
#12593 = CARTESIAN_POINT ( 'NONE',  ( 158.0000000000005400, 153.7952498048169048, 45.00000000000000000 ) ) ;
#12594 = CARTESIAN_POINT ( 'NONE',  ( 115.1311745403725553, 230.6057037040560544, -98.75303131641626919 ) ) ;
#12595 = ORIENTED_EDGE ( 'NONE', *, *, #24398, .T. ) ;
#12596 = VECTOR ( 'NONE', #8610, 1000.000000000000000 ) ;
#12597 = DIRECTION ( 'NONE',  ( 1.000000000000000000, 0.000000000000000000, 0.000000000000000000 ) ) ;
#12598 = CARTESIAN_POINT ( 'NONE',  ( 105.0440993989431604, 246.7662739188597527, -21.68283346401344147 ) ) ;
#12599 = FACE_OUTER_BOUND ( 'NONE', #12466, .T. ) ;
#12600 = DIRECTION ( 'NONE',  ( -1.000000000000000000, -0.000000000000000000, 3.053113317719176147E-15 ) ) ;
#12601 = DIRECTION ( 'NONE',  ( 0.9784193629480814058, 0.2066290158914539099, 0.000000000000000000 ) ) ;
#12602 = AXIS2_PLACEMENT_3D ( 'NONE', #20279, #2313, #2605 ) ;
#12603 = ORIENTED_EDGE ( 'NONE', *, *, #1761, .T. ) ;
#12604 = CARTESIAN_POINT ( 'NONE',  ( -232.6158302464227461, 77.06694679626161815, 15.48771011243863427 ) ) ;
#12605 = VERTEX_POINT ( 'NONE', #19848 ) ;
#12606 = LINE ( 'NONE', #20926, #20881 ) ;
#12607 = ORIENTED_EDGE ( 'NONE', *, *, #4319, .F. ) ;
#12608 = ORIENTED_EDGE ( 'NONE', *, *, #23776, .T. ) ;
#12609 = DIRECTION ( 'NONE',  ( 1.000000000000000000, 0.000000000000000000, 0.000000000000000000 ) ) ;
#12610 = VERTEX_POINT ( 'NONE', #4609 ) ;
#12611 = EDGE_CURVE ( 'NONE', #15968, #1390, #7992, .T. ) ;
#12612 = EDGE_LOOP ( 'NONE', ( #3954, #5839, #7656, #20820 ) ) ;
#12613 = CARTESIAN_POINT ( 'NONE',  ( -175.0000000000000000, -120.0000000000001847, -69.99999999999998579 ) ) ;
#12614 = AXIS2_PLACEMENT_3D ( 'NONE', #13861, #9539, #22610 ) ;
#12615 = LINE ( 'NONE', #16286, #11455 ) ;
#12616 = CARTESIAN_POINT ( 'NONE',  ( 157.9999999999999147, 215.9842499849850697, 45.00000000000000000 ) ) ;
#12617 = EDGE_CURVE ( 'NONE', #20334, #23507, #4759, .T. ) ;
#12618 = EDGE_CURVE ( 'NONE', #3081, #27311, #1021, .T. ) ;
#12619 = ADVANCED_FACE ( 'NONE', ( #3306 ), #14415, .T. ) ;
#12620 = CARTESIAN_POINT ( 'NONE',  ( -149.4366259724174597, 124.9893150903529886, -17.81052309126764754 ) ) ;
#12621 = AXIS2_PLACEMENT_3D ( 'NONE', #5405, #7713, #10007 ) ;
#12622 = CARTESIAN_POINT ( 'NONE',  ( 158.0000000000006253, 146.2716247822957598, -45.00000000000000000 ) ) ;
#12623 = DIRECTION ( 'NONE',  ( 0.000000000000000000, 0.000000000000000000, -1.000000000000000000 ) ) ;
#12624 = CARTESIAN_POINT ( 'NONE',  ( 28.11522373509561845, -43.91897918210346319, 99.74458822874382236 ) ) ;
#12625 = CARTESIAN_POINT ( 'NONE',  ( -217.2920046552164308, 87.79525986223114842, -17.98591562465373173 ) ) ;
#12626 = CARTESIAN_POINT ( 'NONE',  ( 129.3841014818332553, 249.4697745299731935, -142.8785553633037466 ) ) ;
#12627 = CARTESIAN_POINT ( 'NONE',  ( -211.1110268895868671, 87.67313158452103039, 24.45088837201200604 ) ) ;
#12628 = DIRECTION ( 'NONE',  ( -0.000000000000000000, -0.000000000000000000, -1.000000000000000000 ) ) ;
#12629 = DIRECTION ( 'NONE',  ( -1.000000000000000000, -0.000000000000000000, -0.000000000000000000 ) ) ;
#12630 = FACE_BOUND ( 'NONE', #178, .T. ) ;
#12631 = ORIENTED_EDGE ( 'NONE', *, *, #5945, .F. ) ;
#12632 = LINE ( 'NONE', #6150, #23831 ) ;
#12633 = FACE_OUTER_BOUND ( 'NONE', #28395, .T. ) ;
#12634 = DIRECTION ( 'NONE',  ( 0.8660254037844432595, 0.4999999999999919509, -0.000000000000000000 ) ) ;
#12636 = EDGE_LOOP ( 'NONE', ( #23227, #11302 ) ) ;
#12635 = VERTEX_POINT ( 'NONE', #6004 ) ;
#12637 = VECTOR ( 'NONE', #9147, 1000.000000000000000 ) ;
#12638 = AXIS2_PLACEMENT_3D ( 'NONE', #18235, #22397, #11921 ) ;
#12639 = CARTESIAN_POINT ( 'NONE',  ( 91.45931183161239630, 239.6823639899074863, -17.19464119471857089 ) ) ;
#12640 = VERTEX_POINT ( 'NONE', #20418 ) ;
#12641 = EDGE_LOOP ( 'NONE', ( #154, #21722 ) ) ;
#12642 = VECTOR ( 'NONE', #3631, 1000.000000000000000 ) ;
#12643 = ORIENTED_EDGE ( 'NONE', *, *, #1911, .T. ) ;
#12644 = EDGE_CURVE ( 'NONE', #22485, #13260, #9654, .T. ) ;
#12645 = EDGE_CURVE ( 'NONE', #17385, #3706, #14895, .T. ) ;
#12646 = ORIENTED_EDGE ( 'NONE', *, *, #14801, .T. ) ;
#12647 = ORIENTED_EDGE ( 'NONE', *, *, #18001, .F. ) ;
#12648 = ORIENTED_EDGE ( 'NONE', *, *, #10331, .T. ) ;
#12649 = DIRECTION ( 'NONE',  ( 0.9985600561963492439, 0.05364526231778202897, 0.000000000000000000 ) ) ;
#12650 = EDGE_CURVE ( 'NONE', #10435, #20930, #5190, .T. ) ;
#12651 = ADVANCED_FACE ( 'NONE', ( #882 ), #25017, .F. ) ;
#12652 = CARTESIAN_POINT ( 'NONE',  ( -230.8916957670046486, 130.8330661503599117, 5.000000000000002665 ) ) ;
#12653 = AXIS2_PLACEMENT_3D ( 'NONE', #2811, #7133, #16466 ) ;
#12654 = VECTOR ( 'NONE', #100, 1000.000000000000000 ) ;
#12655 = DIRECTION ( 'NONE',  ( -0.000000000000000000, -0.000000000000000000, -1.000000000000000000 ) ) ;
#12656 = CARTESIAN_POINT ( 'NONE',  ( 157.4999999999998010, 236.3011875487955251, -45.00000000000000000 ) ) ;
#12657 = CARTESIAN_POINT ( 'NONE',  ( -210.0000000000000568, -157.0000000000000284, 105.0000000000000284 ) ) ;
#12658 = AXIS2_PLACEMENT_3D ( 'NONE', #13986, #16270, #18555 ) ;
#12659 = PLANE ( 'NONE',  #14183 ) ;
#12660 = CYLINDRICAL_SURFACE ( 'NONE', #19385, 19.99999999999998934 ) ;
#12661 = DIRECTION ( 'NONE',  ( 0.4528218681379515553, 0.8916010070295208312, -0.000000000000000000 ) ) ;
#12662 = CARTESIAN_POINT ( 'NONE',  ( -210.0000000000000568, -152.0000000000000284, -94.99999999999987210 ) ) ;
#12663 = DIRECTION ( 'NONE',  ( -1.321694076934710155E-16, 1.000000000000000000, 0.000000000000000000 ) ) ;
#12664 = DIRECTION ( 'NONE',  ( 1.000000000000000000, 8.313992734408275564E-16, 0.000000000000000000 ) ) ;
#12665 = ORIENTED_EDGE ( 'NONE', *, *, #15982, .T. ) ;
#12666 = CARTESIAN_POINT ( 'NONE',  ( 157.4999999999996305, 288.9665627064425735, 45.00000000000000000 ) ) ;
#12667 = CARTESIAN_POINT ( 'NONE',  ( 158.0000000000011369, 98.11412463215494029, -45.00000000000000000 ) ) ;
#12668 = VERTEX_POINT ( 'NONE', #748 ) ;
#12669 = CIRCLE ( 'NONE', #2103, 68.83858790703926900 ) ;
#12670 = EDGE_CURVE ( 'NONE', #22498, #24909, #24740, .T. ) ;
#12671 = ORIENTED_EDGE ( 'NONE', *, *, #6037, .T. ) ;
#12672 = AXIS2_PLACEMENT_3D ( 'NONE', #9577, #7420, #24659 ) ;
#12673 = AXIS2_PLACEMENT_3D ( 'NONE', #18283, #22736, #20570 ) ;
#12674 = ORIENTED_EDGE ( 'NONE', *, *, #5004, .T. ) ;
#12675 = ADVANCED_FACE ( 'NONE', ( #18551 ), #2894, .F. ) ;
#12676 = CARTESIAN_POINT ( 'NONE',  ( 119.9999999987673220, 136.1131920015923811, 100.0000000000000142 ) ) ;
#12677 = CARTESIAN_POINT ( 'NONE',  ( 11.56692809527929278, 215.3083398198040470, -45.00000000000000000 ) ) ;
#12678 = VERTEX_POINT ( 'NONE', #13980 ) ;
#12679 = AXIS2_PLACEMENT_3D ( 'NONE', #20522, #24840, #22542 ) ;
#12680 = ORIENTED_EDGE ( 'NONE', *, *, #24395, .T. ) ;
#12681 = DIRECTION ( 'NONE',  ( 0.8916010070299876800, -0.4528218681370323462, 0.000000000000000000 ) ) ;
#12682 = CARTESIAN_POINT ( 'NONE',  ( 101.6154567033504748, 236.6169251702747545, 24.17999014744245656 ) ) ;
#12683 = DIRECTION ( 'NONE',  ( -4.625929269271489858E-16, 0.000000000000000000, -1.000000000000000000 ) ) ;
#12684 = VERTEX_POINT ( 'NONE', #27024 ) ;
#12685 = DIRECTION ( 'NONE',  ( -0.000000000000000000, -0.000000000000000000, -1.000000000000000000 ) ) ;
#12686 = ORIENTED_EDGE ( 'NONE', *, *, #26592, .T. ) ;
#12687 = DIRECTION ( 'NONE',  ( -0.4528218681382848443, 0.8916010070293515222, 0.000000000000000000 ) ) ;
#12688 = EDGE_CURVE ( 'NONE', #5617, #25077, #27163, .T. ) ;
#12689 = CARTESIAN_POINT ( 'NONE',  ( -107.3221550338875687, 69.54464929955099706, 80.00000000000001421 ) ) ;
#12690 = LINE ( 'NONE', #18713, #3556 ) ;
#12691 = VECTOR ( 'NONE', #4452, 1000.000000000000114 ) ;
#12692 = CARTESIAN_POINT ( 'NONE',  ( -68.57415822541635464, 24.64876300893806160, 95.00000000000000000 ) ) ;
#12693 = VECTOR ( 'NONE', #16155, 1000.000000000000000 ) ;
#12694 = ORIENTED_EDGE ( 'NONE', *, *, #9629, .T. ) ;
#12695 = CARTESIAN_POINT ( 'NONE',  ( 79.99999999999994316, 80.00000000000001421, 100.0000000000000142 ) ) ;
#12697 = DIRECTION ( 'NONE',  ( 0.8916010070298455714, -0.4528218681373120669, 0.000000000000000000 ) ) ;
#12696 = VECTOR ( 'NONE', #2344, 1000.000000000000227 ) ;
#12698 = PLANE ( 'NONE',  #1902 ) ;
#12699 = DIRECTION ( 'NONE',  ( -0.3102637045530566295, 0.9506505318133544602, 0.000000000000000000 ) ) ;
#12700 = VERTEX_POINT ( 'NONE', #22726 ) ;
#12701 = ADVANCED_FACE ( 'NONE', ( #12633 ), #22859, .T. ) ;
#12702 = DIRECTION ( 'NONE',  ( -0.000000000000000000, 0.000000000000000000, 1.000000000000000000 ) ) ;
#12703 = CARTESIAN_POINT ( 'NONE',  ( 187.4999999999996305, 133.0668745871126930, 36.86484227207694886 ) ) ;
#12704 = CARTESIAN_POINT ( 'NONE',  ( 74.37710191228967460, 227.8920494084358950, 45.00000000000000000 ) ) ;
#12705 = LINE ( 'NONE', #28034, #26370 ) ;
#12706 = ORIENTED_EDGE ( 'NONE', *, *, #6319, .F. ) ;
#12707 = DIRECTION ( 'NONE',  ( 0.000000000000000000, 9.251858538542967883E-17, -1.000000000000000000 ) ) ;
#12708 = ORIENTED_EDGE ( 'NONE', *, *, #15165, .T. ) ;
#12709 = EDGE_CURVE ( 'NONE', #2123, #21119, #9375, .T. ) ;
#12710 = LINE ( 'NONE', #27898, #6960 ) ;
#12711 = CARTESIAN_POINT ( 'NONE',  ( -189.6026171856603355, 103.6733896582188663, -32.02322945567066625 ) ) ;
#12712 = EDGE_LOOP ( 'NONE', ( #15554, #4949, #24625, #20299, #9901, #7409, #3637, #17898, #16548 ) ) ;
#12713 = AXIS2_PLACEMENT_3D ( 'NONE', #20294, #7083, #5059 ) ;
#12714 = ORIENTED_EDGE ( 'NONE', *, *, #10623, .T. ) ;
#12715 = DIRECTION ( 'NONE',  ( -0.000000000000000000, -0.000000000000000000, -1.000000000000000000 ) ) ;
#12716 = ORIENTED_EDGE ( 'NONE', *, *, #8957, .T. ) ;
#12717 = ORIENTED_EDGE ( 'NONE', *, *, #3738, .F. ) ;
#12718 = VERTEX_POINT ( 'NONE', #16404 ) ;
#12719 = PLANE ( 'NONE',  #27654 ) ;
#12720 = EDGE_CURVE ( 'NONE', #12356, #26471, #20841, .T. ) ;
#12721 = ADVANCED_FACE ( 'NONE', ( #3028 ), #7359, .F. ) ;
#12722 = DIRECTION ( 'NONE',  ( -1.000000000000000000, -2.312964634635742957E-16, 0.000000000000000000 ) ) ;
#12723 = CARTESIAN_POINT ( 'NONE',  ( -141.6428522700808230, 17.24192588826928585, 80.00000000000001421 ) ) ;
#12724 = LINE ( 'NONE', #16602, #467 ) ;
#12725 = LINE ( 'NONE', #23484, #19282 ) ;
#12726 = CARTESIAN_POINT ( 'NONE',  ( 157.4999999999998579, 176.1121873686267350, -45.00000000000000000 ) ) ;
#12727 = CARTESIAN_POINT ( 'NONE',  ( -228.8737713456793017, 63.73618850397832603, -17.32239903714437901 ) ) ;
#12728 = ORIENTED_EDGE ( 'NONE', *, *, #24668, .F. ) ;
#12729 = DIRECTION ( 'NONE',  ( -0.000000000000000000, 0.000000000000000000, -1.000000000000000000 ) ) ;
#12730 = CYLINDRICAL_SURFACE ( 'NONE', #25286, 21.59849023212046149 ) ;
#12731 = LINE ( 'NONE', #2071, #10496 ) ;
#12732 = CARTESIAN_POINT ( 'NONE',  ( 112.4997598733875463, 219.4957354009212622, -96.61410599988441561 ) ) ;
#12733 = CIRCLE ( 'NONE', #8601, 35.18636678425507114 ) ;
#12734 = ORIENTED_EDGE ( 'NONE', *, *, #15590, .F. ) ;
#12735 = EDGE_CURVE ( 'NONE', #10893, #553, #7499, .T. ) ;
#12736 = CYLINDRICAL_SURFACE ( 'NONE', #10488, 178.6603051211419597 ) ;
#12737 = CARTESIAN_POINT ( 'NONE',  ( 158.0000000000009379, 118.1771246922112653, 45.00000000000000000 ) ) ;
#12738 = CARTESIAN_POINT ( 'NONE',  ( 154.8288972274760908, 217.3894761555990556, 45.00000000000000000 ) ) ;
#12739 = FACE_OUTER_BOUND ( 'NONE', #25608, .T. ) ;
#12740 = LINE ( 'NONE', #13026, #838 ) ;
#12741 = DIRECTION ( 'NONE',  ( -0.000000000000000000, -0.000000000000000000, 1.000000000000000000 ) ) ;
#12742 = ORIENTED_EDGE ( 'NONE', *, *, #5358, .T. ) ;
#12743 = ADVANCED_FACE ( 'NONE', ( #1160 ), #14250, .F. ) ;
#12744 = ADVANCED_FACE ( 'NONE', ( #21942 ), #10745, .F. ) ;
#12745 = ORIENTED_EDGE ( 'NONE', *, *, #25500, .F. ) ;
#12746 = CARTESIAN_POINT ( 'NONE',  ( 48.74042075079900371, -13.05995637893015449, 45.00000000000000000 ) ) ;
#12747 = ORIENTED_EDGE ( 'NONE', *, *, #1414, .T. ) ;
#12748 = EDGE_CURVE ( 'NONE', #14709, #13208, #26381, .T. ) ;
#12749 = ORIENTED_EDGE ( 'NONE', *, *, #4290, .T. ) ;
#12750 = CARTESIAN_POINT ( 'NONE',  ( -42.65532241761713550, 131.0044336801081784, 16.34779397420838265 ) ) ;
#12751 = VERTEX_POINT ( 'NONE', #8594 ) ;
#12752 = ORIENTED_EDGE ( 'NONE', *, *, #23231, .T. ) ;
#12753 = FACE_BOUND ( 'NONE', #6867, .T. ) ;
#12754 = VECTOR ( 'NONE', #15648, 1000.000000000000000 ) ;
#12755 = CARTESIAN_POINT ( 'NONE',  ( -152.1205167745108326, 122.9384117505879885, -20.31814181434752342 ) ) ;
#12756 = DIRECTION ( 'NONE',  ( 0.4528218681376912080, -0.8916010070296530587, 0.000000000000000000 ) ) ;
#12757 = AXIS2_PLACEMENT_3D ( 'NONE', #25168, #12259, #3326 ) ;
#12758 = CARTESIAN_POINT ( 'NONE',  ( -122.8178735660354306, 132.7857580173457279, -15.82982010538316153 ) ) ;
#12759 = DIRECTION ( 'NONE',  ( 0.8916010070293486356, 0.4528218681382907285, 0.000000000000000000 ) ) ;
#12760 = CARTESIAN_POINT ( 'NONE',  ( -263.5350310235390339, -171.3954706173032321, 89.83034331963602881 ) ) ;
#12761 = CARTESIAN_POINT ( 'NONE',  ( -223.8285381716049187, 88.79728400276415812, -16.70700657864426475 ) ) ;
#12762 = CARTESIAN_POINT ( 'NONE',  ( 131.0364239427135544, 249.7383283561057112, -140.4786076439499709 ) ) ;
#12763 = CARTESIAN_POINT ( 'NONE',  ( -216.0423832044228902, 86.42328519517769791, 21.02196399024839479 ) ) ;
#12764 = DIRECTION ( 'NONE',  ( 0.000000000000000000, 0.000000000000000000, -1.000000000000000000 ) ) ;
#12765 = FACE_OUTER_BOUND ( 'NONE', #11037, .T. ) ;
#12766 = CARTESIAN_POINT ( 'NONE',  ( 157.4999999999997442, 253.8563126013445697, -45.00000000000000000 ) ) ;
#12767 = ORIENTED_EDGE ( 'NONE', *, *, #11587, .F. ) ;
#12768 = AXIS2_PLACEMENT_3D ( 'NONE', #23845, #4006, #12793 ) ;
#12769 = AXIS2_PLACEMENT_3D ( 'NONE', #5363, #3061, #20167 ) ;
#12770 = DIRECTION ( 'NONE',  ( -0.000000000000000000, -0.000000000000000000, 1.000000000000000000 ) ) ;
#12771 = FACE_BOUND ( 'NONE', #9564, .T. ) ;
#12772 = LINE ( 'NONE', #23390, #6488 ) ;
#12774 = VERTEX_POINT ( 'NONE', #8453 ) ;
#12773 = ORIENTED_EDGE ( 'NONE', *, *, #17923, .F. ) ;
#12775 = EDGE_CURVE ( 'NONE', #11684, #15436, #1691, .T. ) ;
#12776 = EDGE_CURVE ( 'NONE', #22333, #13234, #13335, .T. ) ;
#12777 = CARTESIAN_POINT ( 'NONE',  ( 93.75109487930336627, 231.1752187890907351, -18.33298295918092435 ) ) ;
#12778 = VERTEX_POINT ( 'NONE', #19221 ) ;
#12779 = VERTEX_POINT ( 'NONE', #6575 ) ;
#12780 = ORIENTED_EDGE ( 'NONE', *, *, #25957, .F. ) ;
#12781 = VECTOR ( 'NONE', #2687, 1000.000000000000000 ) ;
#12782 = EDGE_LOOP ( 'NONE', ( #24061, #6766, #4033, #12326 ) ) ;
#12783 = VERTEX_POINT ( 'NONE', #19506 ) ;
#12784 = EDGE_LOOP ( 'NONE', ( #1028, #12809, #5058, #22014 ) ) ;
#12785 = CARTESIAN_POINT ( 'NONE',  ( -175.0000000000000000, -120.0000000000001847, -75.99999999999998579 ) ) ;
#12786 = ADVANCED_FACE ( 'NONE', ( #15062 ), #24107, .T. ) ;
#12787 = VECTOR ( 'NONE', #1681, 1000.000000000000114 ) ;
#12788 = CARTESIAN_POINT ( 'NONE',  ( 157.4999999999998295, 228.7775625262745223, -45.00000000000000000 ) ) ;
#12789 = LINE ( 'NONE', #3863, #18530 ) ;
#12790 = CARTESIAN_POINT ( 'NONE',  ( 367.4999999999996021, 44.41075299063184190, 75.00000000000004263 ) ) ;
#12791 = EDGE_CURVE ( 'NONE', #10678, #22419, #28109, .T. ) ;
#12792 = CARTESIAN_POINT ( 'NONE',  ( -260.0000000000001137, -167.0819201924624906, -109.9999999999998721 ) ) ;
#12793 = DIRECTION ( 'NONE',  ( -0.000000000000000000, 0.000000000000000000, -1.000000000000000000 ) ) ;
#12794 = CARTESIAN_POINT ( 'NONE',  ( 157.4999999999997158, 261.3799376238655441, 45.00000000000000000 ) ) ;
#12796 = CARTESIAN_POINT ( 'NONE',  ( -31.54256950484095867, 129.2255411891219978, 16.97092939656602795 ) ) ;
#12795 = AXIS2_PLACEMENT_3D ( 'NONE', #28212, #12597, #21336 ) ;
#12797 = CARTESIAN_POINT ( 'NONE',  ( 20.92655468430566756, 155.3461090732848220, 12.99999999999999822 ) ) ;
#12798 = DIRECTION ( 'NONE',  ( 0.000000000000000000, 0.000000000000000000, 1.000000000000000000 ) ) ;
#12799 = EDGE_CURVE ( 'NONE', #27375, #24009, #15353, .T. ) ;
#12800 = FACE_OUTER_BOUND ( 'NONE', #15751, .T. ) ;
#12801 = ORIENTED_EDGE ( 'NONE', *, *, #12720, .F. ) ;
#12802 = CARTESIAN_POINT ( 'NONE',  ( -162.3832362631574426, 119.5298884965290682, 23.01156641556860549 ) ) ;
#12803 = ADVANCED_FACE ( 'NONE', ( #4549 ), #25967, .F. ) ;
#12804 = AXIS2_PLACEMENT_3D ( 'NONE', #23280, #23142, #5886 ) ;
#12805 = PRODUCT_DEFINITION_SHAPE ( 'NONE', 'NONE',  #28408 ) ;
#12806 = EDGE_CURVE ( 'NONE', #27311, #21270, #19359, .T. ) ;
#12807 = VECTOR ( 'NONE', #17123, 1000.000000000000000 ) ;
#12808 = CARTESIAN_POINT ( 'NONE',  ( -160.0000000000000284, 109.9999999999999432, 100.0000000000000142 ) ) ;
#12809 = ORIENTED_EDGE ( 'NONE', *, *, #10080, .F. ) ;
#12810 = APPLICATION_PROTOCOL_DEFINITION ( 'draft international standard', 'automotive_design', 1998, #14803 ) ;
#12811 = ORIENTED_EDGE ( 'NONE', *, *, #11017, .T. ) ;
#12812 = ORIENTED_EDGE ( 'NONE', *, *, #15839, .F. ) ;
#12813 = CARTESIAN_POINT ( 'NONE',  ( 88.58553289616391169, 111.2425746093149002, 99.99999999998919975 ) ) ;
#12814 = DIRECTION ( 'NONE',  ( -0.000000000000000000, -0.000000000000000000, -1.000000000000000000 ) ) ;
#12815 = VERTEX_POINT ( 'NONE', #23819 ) ;
#12816 = EDGE_LOOP ( 'NONE', ( #16928, #10079, #14793, #19826 ) ) ;
#12817 = CARTESIAN_POINT ( 'NONE',  ( 109.9999999984624850, 137.0808454111539447, -100.0000000001515872 ) ) ;
#12818 = CARTESIAN_POINT ( 'NONE',  ( 95.14885519176667117, 231.7800616880396092, 19.10095409356435070 ) ) ;
#12819 = CONICAL_SURFACE ( 'NONE', #13268, 6.025000000000002132, 0.7853981633974482790 ) ;
#12820 = DIRECTION ( 'NONE',  ( 1.000000000000000000, 1.321694076934710155E-16, -4.625929269271489858E-16 ) ) ;
#12821 = EDGE_LOOP ( 'NONE', ( #14896, #25919, #26165, #13306 ) ) ;
#12822 = CARTESIAN_POINT ( 'NONE',  ( -226.3114843550383171, 89.76160135746334845, 15.90464330981206054 ) ) ;
#12823 = VERTEX_POINT ( 'NONE', #11032 ) ;
#12824 = DIRECTION ( 'NONE',  ( 1.000000000000000000, 8.570722872813602225E-16, 0.000000000000000000 ) ) ;
#12825 = AXIS2_PLACEMENT_3D ( 'NONE', #21690, #26282, #15383 ) ;
#12826 = CARTESIAN_POINT ( 'NONE',  ( 330.9869376377542949, 44.41075299063183479, 100.0000000000000284 ) ) ;
#12827 = CARTESIAN_POINT ( 'NONE',  ( 157.9999999999996589, 273.6653751576470768, 45.00000000000000000 ) ) ;
#12828 = AXIS2_PLACEMENT_3D ( 'NONE', #5599, #23130, #11945 ) ;
#12829 = DIRECTION ( 'NONE',  ( 0.5804519453834686704, -0.8142945039115434547, 0.000000000000000000 ) ) ;
#12830 = EDGE_CURVE ( 'NONE', #7854, #11439, #17193, .T. ) ;
#12831 = EDGE_LOOP ( 'NONE', ( #3627, #21200 ) ) ;
#12832 = CARTESIAN_POINT ( 'NONE',  ( -160.0000000000000284, 59.99999999999994316, 80.00000000000001421 ) ) ;
#12833 = DIRECTION ( 'NONE',  ( 0.4383711467890776259, -5.368498217537984310E-17, 0.8987940462991669266 ) ) ;
#12834 = LINE ( 'NONE', #16852, #15235 ) ;
#12835 = DIRECTION ( 'NONE',  ( -0.8379557447115539848, -0.5457381880580697286, 0.000000000000000000 ) ) ;
#12836 = EDGE_LOOP ( 'NONE', ( #25833, #8726 ) ) ;
#12837 = LINE ( 'NONE', #10954, #10083 ) ;
#12838 = AXIS2_PLACEMENT_3D ( 'NONE', #20103, #24850, #437 ) ;
#12839 = EDGE_CURVE ( 'NONE', #9431, #17312, #4326, .T. ) ;
#12840 = DIRECTION ( 'NONE',  ( -0.000000000000000000, -0.000000000000000000, 1.000000000000000000 ) ) ;
#12841 = DIRECTION ( 'NONE',  ( 0.000000000000000000, 0.000000000000000000, 1.000000000000000000 ) ) ;
#12842 = CARTESIAN_POINT ( 'NONE',  ( -211.7675867465070496, 88.48852952219857571, 21.99030125636233635 ) ) ;
#12843 = ORIENTED_EDGE ( 'NONE', *, *, #18839, .T. ) ;
#12844 = DIRECTION ( 'NONE',  ( -0.8660254037844362651, 0.5000000000000039968, -0.000000000000000000 ) ) ;
#12845 = ORIENTED_EDGE ( 'NONE', *, *, #22607, .T. ) ;
#12846 = AXIS2_PLACEMENT_3D ( 'NONE', #2937, #22480, #24635 ) ;
#12847 = EDGE_CURVE ( 'NONE', #1670, #6691, #17063, .T. ) ;
#12848 = CARTESIAN_POINT ( 'NONE',  ( 157.9999999999996874, 268.6496251426330559, -45.00000000000000000 ) ) ;
#12849 = CARTESIAN_POINT ( 'NONE',  ( -183.1579956025468618, 108.0230262084780435, -31.30096897312795434 ) ) ;
#12850 = ORIENTED_EDGE ( 'NONE', *, *, #20779, .T. ) ;
#12851 = ORIENTED_EDGE ( 'NONE', *, *, #9471, .T. ) ;
#12852 = VECTOR ( 'NONE', #13043, 1000.000000000000000 ) ;
#12853 = DIRECTION ( 'NONE',  ( 0.000000000000000000, 0.000000000000000000, 1.000000000000000000 ) ) ;
#12854 = VERTEX_POINT ( 'NONE', #8731 ) ;
#12855 = EDGE_LOOP ( 'NONE', ( #833, #8787, #2256, #3283 ) ) ;
#12856 = EDGE_LOOP ( 'NONE', ( #18602, #22526, #3601, #1193, #26204, #20323 ) ) ;
#12857 = EDGE_CURVE ( 'NONE', #10473, #25781, #17344, .T. ) ;
#12858 = DIRECTION ( 'NONE',  ( 1.000000000000000000, 0.000000000000000000, -0.000000000000000000 ) ) ;
#12859 = AXIS2_PLACEMENT_3D ( 'NONE', #16463, #27496, #1644 ) ;
#12860 = DIRECTION ( 'NONE',  ( -1.321694076934710155E-16, 1.000000000000000000, 0.000000000000000000 ) ) ;
#12861 = DIRECTION ( 'NONE',  ( 0.000000000000000000, 0.000000000000000000, -1.000000000000000000 ) ) ;
#12862 = PLANE ( 'NONE',  #12215 ) ;
#12863 = CARTESIAN_POINT ( 'NONE',  ( 157.9999999999998010, 236.5551250525490161, -45.00000000000000000 ) ) ;
#12864 = TOROIDAL_SURFACE ( 'NONE', #24329, 18.46313063346208239, 2.000000000000000000 ) ;
#12865 = DIRECTION ( 'NONE',  ( 0.8916010070293783896, -0.4528218681382319422, 0.000000000000000000 ) ) ;
#12866 = EDGE_CURVE ( 'NONE', #8798, #11076, #23963, .T. ) ;
#12867 = CARTESIAN_POINT ( 'NONE',  ( -233.4632575733478745, 77.89441575050611277, -15.30815287833104854 ) ) ;
#12868 = VERTEX_POINT ( 'NONE', #28383 ) ;
#12869 = LINE ( 'NONE', #8552, #10016 ) ;
#12870 = DIRECTION ( 'NONE',  ( 1.000000000000000000, 0.000000000000000000, -0.000000000000000000 ) ) ;
#12871 = CARTESIAN_POINT ( 'NONE',  ( 124.2811822434183284, 467.1080826427131001, -145.0000000000000000 ) ) ;
#12872 = LINE ( 'NONE', #24065, #11666 ) ;
#12873 = ORIENTED_EDGE ( 'NONE', *, *, #22508, .F. ) ;
#12874 = CARTESIAN_POINT ( 'NONE',  ( 0.03735363077137947296, 1.249999999999999556, -7.196572270765070556 ) ) ;
#12875 = CARTESIAN_POINT ( 'NONE',  ( 114.5814157129579058, 230.6339745962151540, 45.00000000000000000 ) ) ;
#12876 = DIRECTION ( 'NONE',  ( 1.541976423090495387E-16, -1.000000000000000000, 0.000000000000000000 ) ) ;
#12877 = CARTESIAN_POINT ( 'NONE',  ( 179.9999999999999147, 330.0000000000000000, -84.99999999999997158 ) ) ;
#12878 = DIRECTION ( 'NONE',  ( -0.8916010070298665546, -0.4528218681372709331, 0.000000000000000000 ) ) ;
#12879 = CARTESIAN_POINT ( 'NONE',  ( 157.4999999999998579, 68.27356204582390831, -45.00000000000000000 ) ) ;
#12880 = ORIENTED_EDGE ( 'NONE', *, *, #13000, .T. ) ;
#12881 = ADVANCED_FACE ( 'NONE', ( #21805, #12771, #2114 ), #19647, .T. ) ;
#12882 = VECTOR ( 'NONE', #13423, 1000.000000000000000 ) ;
#12883 = DIRECTION ( 'NONE',  ( 0.000000000000000000, -1.000000000000000000, 0.000000000000000000 ) ) ;
#12884 = ORIENTED_EDGE ( 'NONE', *, *, #11001, .F. ) ;
#12885 = ADVANCED_FACE ( 'NONE', ( #20212 ), #26961, .F. ) ;
#12886 = CARTESIAN_POINT ( 'NONE',  ( -270.1042321369618548, -170.3737068505718639, 93.67314610463054692 ) ) ;
#12887 = ORIENTED_EDGE ( 'NONE', *, *, #7075, .T. ) ;
#12888 = EDGE_LOOP ( 'NONE', ( #25728, #22124, #28118 ) ) ;
#12889 = FACE_OUTER_BOUND ( 'NONE', #19939, .T. ) ;
#12890 = AXIS2_PLACEMENT_3D ( 'NONE', #14422, #685, #18210 ) ;
#12891 = ORIENTED_EDGE ( 'NONE', *, *, #26834, .T. ) ;
#12892 = ORIENTED_EDGE ( 'NONE', *, *, #4213, .F. ) ;
#12893 = CARTESIAN_POINT ( 'NONE',  ( 158.0000000000000853, 198.4291249324366504, -45.00000000000000000 ) ) ;
#12894 = ADVANCED_FACE ( 'NONE', ( #4976 ), #27100, .F. ) ;
#12895 = DIRECTION ( 'NONE',  ( -1.000000000000000000, 0.000000000000000000, 0.000000000000000000 ) ) ;
#12896 = CARTESIAN_POINT ( 'NONE',  ( 157.4999999999998579, 198.6830624361901414, 45.00000000000000000 ) ) ;
#12897 = EDGE_CURVE ( 'NONE', #9201, #22969, #7292, .T. ) ;
#12898 = CARTESIAN_POINT ( 'NONE',  ( 157.4999999999998579, 173.6043123611196961, -45.00000000000000000 ) ) ;
#12899 = DIRECTION ( 'NONE',  ( -0.000000000000000000, -0.000000000000000000, -1.000000000000000000 ) ) ;
#12900 = CARTESIAN_POINT ( 'NONE',  ( -160.0000000000000284, 59.99999999999994316, 70.00000000000001421 ) ) ;
#12901 = CARTESIAN_POINT ( 'NONE',  ( -268.7977277042236892, -165.3316741299294392, 88.68837795047839734 ) ) ;
#12902 = CARTESIAN_POINT ( 'NONE',  ( -225.0668536777367308, 87.15822506044099782, -16.53154426491069628 ) ) ;
#12903 = VECTOR ( 'NONE', #24552, 1000.000000000000000 ) ;
#12904 = CARTESIAN_POINT ( 'NONE',  ( 131.9890216985461961, 249.8503482187554425, -150.2048413890044287 ) ) ;
#12905 = CARTESIAN_POINT ( 'NONE',  ( 232.4749999999995964, 133.0668745871126930, -30.86484227207697018 ) ) ;
#12906 = EDGE_CURVE ( 'NONE', #17008, #24175, #26824, .T. ) ;
#12907 = PLANE ( 'NONE',  #11554 ) ;
#12908 = DIRECTION ( 'NONE',  ( -0.000000000000000000, 0.000000000000000000, -1.000000000000000000 ) ) ;
#12909 = LINE ( 'NONE', #21654, #7508 ) ;
#12910 = ORIENTED_EDGE ( 'NONE', *, *, #27399, .T. ) ;
#12911 = VECTOR ( 'NONE', #21402, 1000.000000000000000 ) ;
#12912 = CARTESIAN_POINT ( 'NONE',  ( 117.3825211564071225, 140.0000000000000284, 99.73972676668319082 ) ) ;
#12913 = CARTESIAN_POINT ( 'NONE',  ( -175.0000000000000000, -120.0250000000001762, 70.00000000000001421 ) ) ;
#12914 = CARTESIAN_POINT ( 'NONE',  ( 108.2762260028630976, 206.3663779394882170, -150.7983993365949686 ) ) ;
#12915 = ORIENTED_EDGE ( 'NONE', *, *, #7748, .F. ) ;
#12916 = CARTESIAN_POINT ( 'NONE',  ( 88.05061285013169936, 239.8951213614055007, -16.09479252966708529 ) ) ;
#12917 = ORIENTED_EDGE ( 'NONE', *, *, #20897, .T. ) ;
#12918 = CARTESIAN_POINT ( 'NONE',  ( -42.53273978471831640, 130.9733465240572627, -14.93735646117640492 ) ) ;
#12919 = ORIENTED_EDGE ( 'NONE', *, *, #10754, .T. ) ;
#12920 = VERTEX_POINT ( 'NONE', #6995 ) ;
#12921 = AXIS2_PLACEMENT_3D ( 'NONE', #1650, #16751, #12592 ) ;
#12922 = VERTEX_POINT ( 'NONE', #22226 ) ;
#12923 = ORIENTED_EDGE ( 'NONE', *, *, #20084, .F. ) ;
#12924 = VERTEX_POINT ( 'NONE', #17917 ) ;
#12925 = VECTOR ( 'NONE', #17451, 1000.000000000000000 ) ;
#12926 = LINE ( 'NONE', #16940, #16865 ) ;
#12927 = AXIS2_PLACEMENT_3D ( 'NONE', #9160, #19648, #17769 ) ;
#12928 = DIRECTION ( 'NONE',  ( -0.5975062131282553590, 0.8018642810807399268, 0.000000000000000000 ) ) ;
#12929 = CARTESIAN_POINT ( 'NONE',  ( 134.6436608991879496, 206.7391133850113079, -45.00000000000000000 ) ) ;
#12930 = ADVANCED_FACE ( 'NONE', ( #24816 ), #18068, .T. ) ;
#12931 = CARTESIAN_POINT ( 'NONE',  ( 144.9999999999998863, 220.0000000000000284, -119.9999999999999858 ) ) ;
#12932 = DIRECTION ( 'NONE',  ( 0.8660254037844324904, -0.5000000000000105471, 0.000000000000000000 ) ) ;
#12933 = DIRECTION ( 'NONE',  ( 0.4528218681383106015, 0.8916010070293384215, -0.000000000000000000 ) ) ;
#12934 = CARTESIAN_POINT ( 'NONE',  ( 158.0000000000005684, 153.2873747973098659, 45.00000000000000000 ) ) ;
#12935 = CARTESIAN_POINT ( 'NONE',  ( 153.4775906502255509, 227.6536686473015436, -45.00000000000000000 ) ) ;
#12936 = CIRCLE ( 'NONE', #14783, 5.999999999999991118 ) ;
#12937 = DIRECTION ( 'NONE',  ( 1.000000000000000000, -0.000000000000000000, -0.000000000000000000 ) ) ;
#12938 = DIRECTION ( 'NONE',  ( 0.000000000000000000, 1.000000000000000000, 0.000000000000000000 ) ) ;
#12939 = CARTESIAN_POINT ( 'NONE',  ( 158.0000000000000853, 200.9369999399436892, -45.00000000000000000 ) ) ;
#12940 = CARTESIAN_POINT ( 'NONE',  ( -175.8417606860892874, 246.9430296707336652, 12.99999999999999822 ) ) ;
#12941 = VECTOR ( 'NONE', #15427, 1000.000000000000000 ) ;
#12943 = VERTEX_POINT ( 'NONE', #26668 ) ;
#12942 = EDGE_LOOP ( 'NONE', ( #11819, #21849, #23331, #17844 ) ) ;
#12944 = PRODUCT_DEFINITION_FORMATION_WITH_SPECIFIED_SOURCE ( 'ANY', '', #21502, .NOT_KNOWN. ) ;
#12945 = CARTESIAN_POINT ( 'NONE',  ( -185.8734447760280091, 106.0260592552631635, 32.44447814219098802 ) ) ;
#12946 = VECTOR ( 'NONE', #13441, 1000.000000000000114 ) ;
#12947 = CARTESIAN_POINT ( 'NONE',  ( -272.8482960613322348, -165.2072238553256227, -108.3495407332041651 ) ) ;
#12948 = ORIENTED_EDGE ( 'NONE', *, *, #406, .F. ) ;
#12949 = SHAPE_DEFINITION_REPRESENTATION ( #27675, #22013 ) ;
#12950 = ORIENTED_EDGE ( 'NONE', *, *, #7155, .T. ) ;
#12951 = VERTEX_POINT ( 'NONE', #13475 ) ;
#12952 = CARTESIAN_POINT ( 'NONE',  ( -225.9729034214362855, 132.4331356209112300, -12.99353264133693742 ) ) ;
#12953 = EDGE_CURVE ( 'NONE', #301, #12291, #2532, .T. ) ;
#12954 = CARTESIAN_POINT ( 'NONE',  ( 157.4999999999998579, 173.6043123611196961, 45.00000000000000000 ) ) ;
#12955 = ORIENTED_EDGE ( 'NONE', *, *, #22916, .F. ) ;
#12956 = ORIENTED_EDGE ( 'NONE', *, *, #15210, .T. ) ;
#12957 = CARTESIAN_POINT ( 'NONE',  ( 79.99999999999991473, 110.0000000000000142, -100.0000000000000142 ) ) ;
#12958 = CIRCLE ( 'NONE', #5157, 72.21503689626329958 ) ;
#12960 = DIRECTION ( 'NONE',  ( -1.000000000000000000, 0.000000000000000000, 0.000000000000000000 ) ) ;
#12959 =( REPRESENTATION_RELATIONSHIP ('NONE','NONE', #11963, #14145 ) REPRESENTATION_RELATIONSHIP_WITH_TRANSFORMATION ( #4163 )SHAPE_REPRESENTATION_RELATIONSHIP( ) );
#12961 = LINE ( 'NONE', #14973, #12365 ) ;
#12962 = ORIENTED_EDGE ( 'NONE', *, *, #4216, .F. ) ;
#12963 = EDGE_CURVE ( 'NONE', #12180, #3701, #20065, .T. ) ;
#12964 = CARTESIAN_POINT ( 'NONE',  ( -227.5151209178948477, 90.37154496853476360, 15.60286242741050700 ) ) ;
#12965 = ORIENTED_EDGE ( 'NONE', *, *, #21453, .T. ) ;
#12966 = CIRCLE ( 'NONE', #6528, 16.07743405327025243 ) ;
#12967 = CARTESIAN_POINT ( 'NONE',  ( -220.5365384948381120, 71.33200643684088504, 21.30906822952360358 ) ) ;
#12968 = PLANE ( 'NONE',  #4288 ) ;
#12969 = ADVANCED_FACE ( 'NONE', ( #26520 ), #22665, .F. ) ;
#12970 = AXIS2_PLACEMENT_3D ( 'NONE', #3215, #5938, #12707 ) ;
#12971 = EDGE_CURVE ( 'NONE', #9432, #21245, #4833, .T. ) ;
#12972 = EDGE_CURVE ( 'NONE', #9172, #9499, #6852, .T. ) ;
#12973 = CARTESIAN_POINT ( 'NONE',  ( -248.1546605714623013, -91.18033988749901653, 0.000000000000000000 ) ) ;
#12974 = DIRECTION ( 'NONE',  ( -0.000000000000000000, 0.000000000000000000, 1.000000000000000000 ) ) ;
#12975 = CARTESIAN_POINT ( 'NONE',  ( 158.0000000000010800, 101.1298746471690038, -45.00000000000000000 ) ) ;
#12976 = ORIENTED_EDGE ( 'NONE', *, *, #8640, .F. ) ;
#12977 = DIRECTION ( 'NONE',  ( 0.000000000000000000, 0.000000000000000000, -1.000000000000000000 ) ) ;
#12978 = DIRECTION ( 'NONE',  ( -0.8916010070293383105, -0.4528218681383106015, 0.000000000000000000 ) ) ;
#12979 = DIRECTION ( 'NONE',  ( 1.000000000000000000, 0.000000000000000000, 0.000000000000000000 ) ) ;
#12980 = CARTESIAN_POINT ( 'NONE',  ( 147.1752285801741493, 235.8670668058244644, -45.00000000000000000 ) ) ;
#12981 = ORIENTED_EDGE ( 'NONE', *, *, #8195, .F. ) ;
#12982 = VECTOR ( 'NONE', #27867, 1000.000000000000000 ) ;
#12983 = FACE_OUTER_BOUND ( 'NONE', #4588, .T. ) ;
#12984 = AXIS2_PLACEMENT_3D ( 'NONE', #18101, #13804, #7326 ) ;
#12985 = DIRECTION ( 'NONE',  ( 0.000000000000000000, 0.000000000000000000, 1.000000000000000000 ) ) ;
#12986 = DIRECTION ( 'NONE',  ( 1.000000000000000000, 0.000000000000000000, 0.000000000000000000 ) ) ;
#12987 = CARTESIAN_POINT ( 'NONE',  ( -204.2392738945716530, 92.18060771344825355, 28.15437548428747405 ) ) ;
#12988 = ORIENTED_EDGE ( 'NONE', *, *, #12857, .T. ) ;
#12989 = DIRECTION ( 'NONE',  ( -0.8916010070295816714, 0.4528218681378317068, 0.000000000000000000 ) ) ;
#12990 = VECTOR ( 'NONE', #27361, 1000.000000000000000 ) ;
#12991 = VERTEX_POINT ( 'NONE', #4688 ) ;
#12992 = VECTOR ( 'NONE', #27374, 1000.000000000000114 ) ;
#12993 = LINE ( 'NONE', #2048, #23949 ) ;
#12994 = CARTESIAN_POINT ( 'NONE',  ( -173.5201714974283220, 113.8162285326356198, -26.99751449988017882 ) ) ;
#12995 = ORIENTED_EDGE ( 'NONE', *, *, #6567, .F. ) ;
#12996 = EDGE_LOOP ( 'NONE', ( #16695, #936, #3006, #8877 ) ) ;
#12997 = CARTESIAN_POINT ( 'NONE',  ( -112.1757387330262645, 70.43811608390225842, 82.87215587302765130 ) ) ;
#12998 = EDGE_CURVE ( 'NONE', #12262, #25868, #2823, .T. ) ;
#12999 = VERTEX_POINT ( 'NONE', #2969 ) ;
#13000 = EDGE_CURVE ( 'NONE', #7514, #19329, #822, .T. ) ;
#13001 = LINE ( 'NONE', #15571, #14391 ) ;
#13002 = ORIENTED_EDGE ( 'NONE', *, *, #25566, .F. ) ;
#13003 = ORIENTED_EDGE ( 'NONE', *, *, #23739, .F. ) ;
#13004 = VECTOR ( 'NONE', #770, 1000.000000000000000 ) ;
#13005 = CARTESIAN_POINT ( 'NONE',  ( 158.0000000000014779, 65.51174953456337846, 45.00000000000000000 ) ) ;
#13006 = VECTOR ( 'NONE', #4051, 1000.000000000000114 ) ;
#13007 = EDGE_CURVE ( 'NONE', #2948, #15785, #14441, .T. ) ;
#13008 = DIRECTION ( 'NONE',  ( 0.9659258262890670910, 0.2588190451025251804, 0.000000000000000000 ) ) ;
#13009 = DIRECTION ( 'NONE',  ( 0.7440215159219069063, 0.6681556583950086781, 0.000000000000000000 ) ) ;
#13010 = DIRECTION ( 'NONE',  ( -0.000000000000000000, -0.000000000000000000, 1.000000000000000000 ) ) ;
#13011 = VECTOR ( 'NONE', #1825, 999.9999999999998863 ) ;
#13012 = DIRECTION ( 'NONE',  ( 0.8916010070293783896, -0.4528218681382319422, 0.000000000000000000 ) ) ;
#13013 = CARTESIAN_POINT ( 'NONE',  ( 158.0000000000000853, 198.9369999399436892, 45.00000000000000000 ) ) ;
#13014 = CARTESIAN_POINT ( 'NONE',  ( -227.3197243376772860, 73.27520359174637576, -17.23934621637404163 ) ) ;
#13015 = ADVANCED_FACE ( 'NONE', ( #20359 ), #687, .F. ) ;
#13016 = VERTEX_POINT ( 'NONE', #24954 ) ;
#13017 = DIRECTION ( 'NONE',  ( -1.000000000000000000, 0.000000000000000000, 0.000000000000000000 ) ) ;
#13018 = CARTESIAN_POINT ( 'NONE',  ( -175.0000000000000000, -150.0000000000000853, -64.00000000000000000 ) ) ;
#13019 = DIRECTION ( 'NONE',  ( -0.8916010070294497769, 0.4528218681380914989, 0.000000000000000000 ) ) ;
#13020 = CARTESIAN_POINT ( 'NONE',  ( 112.5876798426281482, 217.9501953190548988, -96.71269508460397901 ) ) ;
#13021 = ORIENTED_EDGE ( 'NONE', *, *, #13845, .T. ) ;
#13022 = DIRECTION ( 'NONE',  ( 0.000000000000000000, 0.000000000000000000, 1.000000000000000000 ) ) ;
#13023 = CARTESIAN_POINT ( 'NONE',  ( -50.01279441628821587, 86.62470095750859400, -45.00000000000000000 ) ) ;
#13024 = PLANE ( 'NONE',  #19247 ) ;
#13025 = DIRECTION ( 'NONE',  ( 0.000000000000000000, 0.000000000000000000, -1.000000000000000000 ) ) ;
#13026 = CARTESIAN_POINT ( 'NONE',  ( 158.0000000000013642, 76.05112457209858690, -45.00000000000000000 ) ) ;
#13027 = ORIENTED_EDGE ( 'NONE', *, *, #16682, .T. ) ;
#13028 = CIRCLE ( 'NONE', #630, 4.999999999999992895 ) ;
#13029 = VECTOR ( 'NONE', #20858, 999.9999999999998863 ) ;
#13030 = DIRECTION ( 'NONE',  ( 0.000000000000000000, -0.000000000000000000, -1.000000000000000000 ) ) ;
#13031 = ORIENTED_EDGE ( 'NONE', *, *, #2403, .T. ) ;
#13032 = CARTESIAN_POINT ( 'NONE',  ( -25.39999999999996305, 0.000000000000000000, 0.000000000000000000 ) ) ;
#13033 = VERTEX_POINT ( 'NONE', #2389 ) ;
#13034 = VECTOR ( 'NONE', #13294, 1000.000000000000000 ) ;
#13035 = ORIENTED_EDGE ( 'NONE', *, *, #26114, .F. ) ;
#13036 = DIRECTION ( 'NONE',  ( 0.8916010070299070778, 0.4528218681371909971, 0.000000000000000000 ) ) ;
#13037 = ADVANCED_FACE ( 'NONE', ( #11172 ), #19927, .F. ) ;
#13038 = EDGE_LOOP ( 'NONE', ( #11623, #22840, #24480, #27243, #12079, #11263 ) ) ;
#13039 = ORIENTED_EDGE ( 'NONE', *, *, #23843, .F. ) ;
#13040 = DIRECTION ( 'NONE',  ( 0.000000000000000000, 0.000000000000000000, -1.000000000000000000 ) ) ;
#13041 = CARTESIAN_POINT ( 'NONE',  ( 0.3651377029009472697, 0.000000000000000000, 0.000000000000000000 ) ) ;
#13042 = CARTESIAN_POINT ( 'NONE',  ( -211.7958164186347574, -218.9496041985363490, 92.43018420650685130 ) ) ;
#13043 = DIRECTION ( 'NONE',  ( -0.000000000000000000, -0.000000000000000000, 1.000000000000000000 ) ) ;
#13044 = DIRECTION ( 'NONE',  ( 0.000000000000000000, 0.000000000000000000, 1.000000000000000000 ) ) ;
#13045 = CARTESIAN_POINT ( 'NONE',  ( -279.3160071107327553, -512.7211954420570237, 0.000000000000000000 ) ) ;
#13046 = DIRECTION ( 'NONE',  ( -0.8916010070299376089, -0.4528218681371311005, 0.000000000000000000 ) ) ;
#13047 = CARTESIAN_POINT ( 'NONE',  ( -219.2341581334216301, 87.88245300808631555, -16.82493878253857034 ) ) ;
#13048 = ADVANCED_FACE ( 'NONE', ( #21197 ), #22803, .F. ) ;
#13049 = PRODUCT_DEFINITION_SHAPE ( 'NONE', 'NONE',  #28405 ) ;
#13050 = EDGE_CURVE ( 'NONE', #10749, #19092, #17671, .T. ) ;
#13051 = DIRECTION ( 'NONE',  ( 1.000000000000000000, 0.000000000000000000, -0.000000000000000000 ) ) ;
#13052 = DIRECTION ( 'NONE',  ( -0.000000000000000000, -0.000000000000000000, 1.000000000000000000 ) ) ;
#13053 = CIRCLE ( 'NONE', #12602, 58.59270260175150469 ) ;
#13054 = DIRECTION ( 'NONE',  ( 0.000000000000000000, 0.000000000000000000, 1.000000000000000000 ) ) ;
#13055 = CARTESIAN_POINT ( 'NONE',  ( 158.0000000000000000, 208.4606249624626457, -45.00000000000000000 ) ) ;
#13056 = CARTESIAN_POINT ( 'NONE',  ( -279.3160071107327553, -98.68033988749907337, 0.000000000000000000 ) ) ;
#13057 = EDGE_LOOP ( 'NONE', ( #9121, #5702, #26427, #14331, #24298 ) ) ;
#13058 = CARTESIAN_POINT ( 'NONE',  ( -160.0000000000000284, 221.6666220619077876, -13.00000000000000000 ) ) ;
#13059 = DIRECTION ( 'NONE',  ( 0.000000000000000000, 0.000000000000000000, 1.000000000000000000 ) ) ;
#13060 = CARTESIAN_POINT ( 'NONE',  ( 119.9999999999999289, 110.0000000000000142, 100.0000000000000142 ) ) ;
#13061 = CARTESIAN_POINT ( 'NONE',  ( 109.0192378864665557, 205.0000000000002558, -138.9999999999999432 ) ) ;
#13062 = ORIENTED_EDGE ( 'NONE', *, *, #2401, .F. ) ;
#13063 = EDGE_CURVE ( 'NONE', #4583, #28122, #19045, .T. ) ;
#13064 = EDGE_CURVE ( 'NONE', #21431, #10405, #3242, .T. ) ;
#13065 = CARTESIAN_POINT ( 'NONE',  ( 94.60831035304303782, 240.0858928317209688, -18.63379520591212213 ) ) ;
#13066 = ORIENTED_EDGE ( 'NONE', *, *, #9378, .F. ) ;
#13067 = LINE ( 'NONE', #4555, #15529 ) ;
#13068 = ORIENTED_EDGE ( 'NONE', *, *, #22265, .T. ) ;
#13069 = AXIS2_PLACEMENT_3D ( 'NONE', #457, #28302, #15689 ) ;
#13070 = ORIENTED_EDGE ( 'NONE', *, *, #17239, .T. ) ;
#13071 = ORIENTED_EDGE ( 'NONE', *, *, #7356, .F. ) ;
#13072 = ORIENTED_EDGE ( 'NONE', *, *, #20910, .F. ) ;
#13073 = DIRECTION ( 'NONE',  ( 1.000000000000000000, 0.000000000000000000, 0.000000000000000000 ) ) ;
#13074 = CARTESIAN_POINT ( 'NONE',  ( 156.4999999999998579, 220.0000000000000284, -99.00000000000001421 ) ) ;
#13075 = DIRECTION ( 'NONE',  ( 0.000000000000000000, 1.000000000000000000, 0.000000000000000000 ) ) ;
#13076 = DIRECTION ( 'NONE',  ( -0.000000000000000000, 0.000000000000000000, -1.000000000000000000 ) ) ;
#13077 = EDGE_CURVE ( 'NONE', #24186, #3711, #16618, .T. ) ;
#13078 = DIRECTION ( 'NONE',  ( -0.000000000000000000, -0.000000000000000000, -1.000000000000000000 ) ) ;
#13079 = CARTESIAN_POINT ( 'NONE',  ( 128.0812361363530272, 198.0425250404537394, 45.00000000000000000 ) ) ;
#13080 = EDGE_CURVE ( 'NONE', #5588, #21528, #7571, .T. ) ;
#13081 = CARTESIAN_POINT ( 'NONE',  ( 167.4999999999996589, 494.4107529906318632, 74.99999999999995737 ) ) ;
#13082 = DIRECTION ( 'NONE',  ( -0.000000000000000000, -0.000000000000000000, 1.000000000000000000 ) ) ;
#13083 = DIRECTION ( 'NONE',  ( 0.8916010070296936929, -0.4528218681376112165, 0.000000000000000000 ) ) ;
#13084 = CARTESIAN_POINT ( 'NONE',  ( -229.0203060419763972, 74.22047013562770701, -16.53676392287966479 ) ) ;
#13085 = AXIS2_PLACEMENT_3D ( 'NONE', #10771, #20382, #18517 ) ;
#13086 = FACE_OUTER_BOUND ( 'NONE', #15291, .T. ) ;
#13087 = CARTESIAN_POINT ( 'NONE',  ( -210.0005531657457425, 60.15481638329399061, 20.01096819387401737 ) ) ;
#13088 = DIRECTION ( 'NONE',  ( 1.000000000000000000, -0.000000000000000000, -0.000000000000000000 ) ) ;
#13089 = CARTESIAN_POINT ( 'NONE',  ( 65.00000000000000000, -120.0250000000000625, 76.00000000000002842 ) ) ;
#13090 = VECTOR ( 'NONE', #13839, 1000.000000000000000 ) ;
#13092 = ORIENTED_EDGE ( 'NONE', *, *, #3117, .F. ) ;
#13091 = EDGE_LOOP ( 'NONE', ( #15791, #25149, #22914, #18384, #11365, #9029 ) ) ;
#13093 = EDGE_CURVE ( 'NONE', #1111, #22350, #18903, .T. ) ;
#13094 = CARTESIAN_POINT ( 'NONE',  ( -160.0000000000000568, 119.7660240611718763, 22.85081902853004010 ) ) ;
#13095 = CARTESIAN_POINT ( 'NONE',  ( 157.9999999999997158, 261.6338751276190351, -45.00000000000000000 ) ) ;
#13096 = EDGE_LOOP ( 'NONE', ( #19121, #9417, #15538, #6122 ) ) ;
#13097 = ITEM_DEFINED_TRANSFORMATION ( 'NONE', 'NONE', #1462,  #10637 ) ;
#13098 = EDGE_LOOP ( 'NONE', ( #7268, #20772, #24016, #12891 ) ) ;
#13099 = EDGE_CURVE ( 'NONE', #12217, #25416, #6178, .T. ) ;
#13101 = EDGE_CURVE ( 'NONE', #22209, #9386, #16757, .T. ) ;
#13100 = ORIENTED_EDGE ( 'NONE', *, *, #1442, .F. ) ;
#13102 = CARTESIAN_POINT ( 'NONE',  ( 217.4999999999996305, 83.06687458711267880, -36.86484227207694175 ) ) ;
#13103 = DIRECTION ( 'NONE',  ( -1.000000000000000000, 0.000000000000000000, 0.000000000000000000 ) ) ;
#13104 = EDGE_LOOP ( 'NONE', ( #10195, #7757, #6501, #4021 ) ) ;
#13105 = VECTOR ( 'NONE', #22649, 1000.000000000000000 ) ;
#13106 = EDGE_CURVE ( 'NONE', #15738, #27472, #22703, .T. ) ;
#13107 = CIRCLE ( 'NONE', #7584, 5.999999999999977796 ) ;
#13108 = VECTOR ( 'NONE', #15199, 1000.000000000000227 ) ;
#13109 = CARTESIAN_POINT ( 'NONE',  ( 90.17595424778114932, 111.7661400906783626, -100.0000000000108571 ) ) ;
#13110 = DIRECTION ( 'NONE',  ( -0.8916010070294909662, -0.4528218681380102306, 0.000000000000000000 ) ) ;
#13111 = ORIENTED_EDGE ( 'NONE', *, *, #18015, .T. ) ;
#13112 = CARTESIAN_POINT ( 'NONE',  ( -228.1049675858170076, 88.39191058023563130, 15.64816112534147763 ) ) ;
#13113 = ORIENTED_EDGE ( 'NONE', *, *, #3152, .F. ) ;
#13114 = VECTOR ( 'NONE', #2287, 999.9999999999998863 ) ;
#13115 = CARTESIAN_POINT ( 'NONE',  ( -210.4359063544881394, -219.8547609215023897, 108.8564660827533999 ) ) ;
#13116 = FACE_OUTER_BOUND ( 'NONE', #20990, .T. ) ;
#13117 = CARTESIAN_POINT ( 'NONE',  ( 157.9841506265077555, 200.7184471377001103, -148.0084258618598199 ) ) ;
#13118 = ORIENTED_EDGE ( 'NONE', *, *, #26899, .T. ) ;
#13119 = CARTESIAN_POINT ( 'NONE',  ( 119.9999999999999147, 203.2294901687515676, 100.0000000000000142 ) ) ;
#13120 = VECTOR ( 'NONE', #7237, 1000.000000000000000 ) ;
#13121 = DIRECTION ( 'NONE',  ( -0.9784193629480845145, -0.2066290158914390329, 0.000000000000000000 ) ) ;
#13122 = DIRECTION ( 'NONE',  ( 1.000000000000000000, 0.000000000000000000, 0.000000000000000000 ) ) ;
#13123 = CARTESIAN_POINT ( 'NONE',  ( 432.4999999999996589, 19.41075299063184900, 80.49671038392669686 ) ) ;
#13124 = AXIS2_PLACEMENT_3D ( 'NONE', #3515, #15016, #23767 ) ;
#13125 = VERTEX_POINT ( 'NONE', #23356 ) ;
#13126 = VECTOR ( 'NONE', #13843, 1000.000000000000114 ) ;
#13127 = CARTESIAN_POINT ( 'NONE',  ( 158.0000000000012506, 86.08262460212675649, -45.00000000000000000 ) ) ;
#13128 = DIRECTION ( 'NONE',  ( 0.8916010070293383105, -0.4528218681383106015, 0.000000000000000000 ) ) ;
#13129 = LINE ( 'NONE', #14858, #22261 ) ;
#13130 = VERTEX_POINT ( 'NONE', #18489 ) ;
#13131 =( NAMED_UNIT ( * ) SI_UNIT ( $, .STERADIAN. ) SOLID_ANGLE_UNIT ( ) );
#13132 = EDGE_CURVE ( 'NONE', #410, #21206, #3386, .T. ) ;
#13133 = CIRCLE ( 'NONE', #23230, 5.999999999999991118 ) ;
#13134 = ORIENTED_EDGE ( 'NONE', *, *, #25587, .F. ) ;
#13135 = EDGE_CURVE ( 'NONE', #19520, #19302, #20774, .T. ) ;
#13136 = CARTESIAN_POINT ( 'NONE',  ( 217.4999999999996305, 258.6181251126050711, 1.387778780781445676E-14 ) ) ;
#13137 = EDGE_CURVE ( 'NONE', #8240, #9208, #14054, .T. ) ;
#13138 = CARTESIAN_POINT ( 'NONE',  ( -189.5865564510991703, 103.6848570016005056, -32.44697421272680060 ) ) ;
#13139 = ORIENTED_EDGE ( 'NONE', *, *, #10390, .T. ) ;
#13140 = VERTEX_POINT ( 'NONE', #3100 ) ;
#13141 = CARTESIAN_POINT ( 'NONE',  ( -113.4248494255375164, 71.17701621305222659, 82.82902054666689651 ) ) ;
#13142 = FACE_OUTER_BOUND ( 'NONE', #19737, .T. ) ;
#13143 = ORIENTED_EDGE ( 'NONE', *, *, #24736, .F. ) ;
#13144 = ORIENTED_EDGE ( 'NONE', *, *, #8181, .F. ) ;
#13145 = AXIS2_PLACEMENT_3D ( 'NONE', #4739, #20113, #13668 ) ;
#13146 = CARTESIAN_POINT ( 'NONE',  ( -175.0000000000000000, -120.0000000000001705, 76.00000000000001421 ) ) ;
#13147 = DIRECTION ( 'NONE',  ( -0.7440215159218921404, 0.6681556583950252204, 0.000000000000000000 ) ) ;
#13148 = PLANE ( 'NONE',  #10286 ) ;
#13149 = CARTESIAN_POINT ( 'NONE',  ( 0.3651377028998192276, -1.249999999999998890, -7.402212548648222423 ) ) ;
#13150 = VECTOR ( 'NONE', #3235, 999.9999999999998863 ) ;
#13151 = CARTESIAN_POINT ( 'NONE',  ( 119.1329331941752230, 232.1752285801739220, 45.00000000000000000 ) ) ;
#13152 = CARTESIAN_POINT ( 'NONE',  ( -209.9392232950165749, 62.66904268397140498, -27.74475063248219087 ) ) ;
#13153 = CARTESIAN_POINT ( 'NONE',  ( 158.0000000000009663, 115.6692496847042264, 45.00000000000000000 ) ) ;
#13154 = ORIENTED_EDGE ( 'NONE', *, *, #8546, .T. ) ;
#13155 = CARTESIAN_POINT ( 'NONE',  ( 157.9999999999997726, 241.5708750675630370, 45.00000000000000000 ) ) ;
#13156 = DIRECTION ( 'NONE',  ( 1.000000000000000000, -0.000000000000000000, -0.000000000000000000 ) ) ;
#13157 = PLANE ( 'NONE',  #24255 ) ;
#13158 = DIRECTION ( 'NONE',  ( 0.8916010070296632728, -0.4528218681376712240, 0.000000000000000000 ) ) ;
#13159 = ORIENTED_EDGE ( 'NONE', *, *, #1454, .T. ) ;
#13160 = CARTESIAN_POINT ( 'NONE',  ( -290.0000000000001137, -157.0000000000000284, 60.00000000000002842 ) ) ;
#13161 = DIRECTION ( 'NONE',  ( 0.5555587585212683477, 0.8314772792026894344, -0.000000000000000000 ) ) ;
#13162 = CARTESIAN_POINT ( 'NONE',  ( 89.99999999999994316, -90.00000000000001421, -100.0000000000000142 ) ) ;
#13163 = DIRECTION ( 'NONE',  ( -0.000000000000000000, -0.000000000000000000, 1.000000000000000000 ) ) ;
#13164 = CARTESIAN_POINT ( 'NONE',  ( 158.0000000000001990, 186.3976249024084666, 45.00000000000000000 ) ) ;
#13165 = CARTESIAN_POINT ( 'NONE',  ( 157.9999999999996589, 278.6811251726610976, 45.00000000000000000 ) ) ;
#13166 = ORIENTED_EDGE ( 'NONE', *, *, #8571, .F. ) ;
#13167 = VECTOR ( 'NONE', #12715, 1000.000000000000000 ) ;
#13168 = ADVANCED_FACE ( 'NONE', ( #11896 ), #25093, .T. ) ;
#13169 = CARTESIAN_POINT ( 'NONE',  ( 432.4999999999996589, -5.589247009368160768, 100.0000000000000426 ) ) ;
#13170 = EDGE_LOOP ( 'NONE', ( #8051, #13510, #8803, #12995 ) ) ;
#13171 = ADVANCED_FACE ( 'NONE', ( #12599 ), #1583, .T. ) ;
#13172 = CARTESIAN_POINT ( 'NONE',  ( 158.0000000000015064, 63.00387452705633251, -45.00000000000000000 ) ) ;
#13173 = VERTEX_POINT ( 'NONE', #6252 ) ;
#13174 = ORIENTED_EDGE ( 'NONE', *, *, #4602, .T. ) ;
#13175 = CARTESIAN_POINT ( 'NONE',  ( 157.9999999999997158, 261.1260001201120531, 45.00000000000000000 ) ) ;
#13176 = PRODUCT_DEFINITION ( 'UNKNOWN', '', #14340, #24688 ) ;
#13177 = EDGE_LOOP ( 'NONE', ( #28190, #16968, #14734, #2425 ) ) ;
#13178 = ORIENTED_EDGE ( 'NONE', *, *, #18949, .T. ) ;
#13179 = CARTESIAN_POINT ( 'NONE',  ( -189.8086322075389774, 92.49158130768422836, -15.00000000000000000 ) ) ;
#13180 = CARTESIAN_POINT ( 'NONE',  ( 89.37316688736845549, 230.0797033051429707, 16.48577246127769058 ) ) ;
#13181 = DIRECTION ( 'NONE',  ( 1.000000000000000000, -0.000000000000000000, -0.000000000000000000 ) ) ;
#13182 = CARTESIAN_POINT ( 'NONE',  ( 157.4999999999998579, 151.0334372935563465, 45.00000000000000000 ) ) ;
#13183 = VECTOR ( 'NONE', #2443, 1000.000000000000000 ) ;
#13184 = LINE ( 'NONE', #13322, #16528 ) ;
#13185 = CARTESIAN_POINT ( 'NONE',  ( 157.4999999999998579, 141.0019372635281627, 45.00000000000000000 ) ) ;
#13186 = PLANE ( 'NONE',  #6978 ) ;
#13187 = CARTESIAN_POINT ( 'NONE',  ( 157.9999999999998579, 223.5078750075070104, 45.00000000000000000 ) ) ;
#13188 = LINE ( 'NONE', #8444, #21809 ) ;
#13189 = EDGE_CURVE ( 'NONE', #3105, #26789, #15029, .T. ) ;
#13190 = DIRECTION ( 'NONE',  ( -0.000000000000000000, 0.000000000000000000, -1.000000000000000000 ) ) ;
#13191 = CARTESIAN_POINT ( 'NONE',  ( 158.0000000000005400, 158.3031248123239436, -45.00000000000000000 ) ) ;
#13192 = CARTESIAN_POINT ( 'NONE',  ( -124.9781469243919076, 222.2250949724356985, 15.00000000000000000 ) ) ;
#13193 = VERTEX_POINT ( 'NONE', #4094 ) ;
#13194 = ADVANCED_FACE ( 'NONE', ( #12739 ), #1793, .F. ) ;
#13195 = DIRECTION ( 'NONE',  ( 0.000000000000000000, -1.000000000000000000, 0.000000000000000000 ) ) ;
#13196 = DIRECTION ( 'NONE',  ( -0.000000000000000000, -0.000000000000000000, 1.000000000000000000 ) ) ;
#13197 = CARTESIAN_POINT ( 'NONE',  ( 107.0542349192081275, 209.0860837716736000, -141.0358260266775972 ) ) ;
#13198 = ORIENTED_EDGE ( 'NONE', *, *, #20310, .F. ) ;
#13199 = DIRECTION ( 'NONE',  ( 0.4528218681382319422, 0.8916010070293783896, -0.000000000000000000 ) ) ;
#13200 = ORIENTED_EDGE ( 'NONE', *, *, #8219, .T. ) ;
#13201 = EDGE_CURVE ( 'NONE', #18699, #26642, #18108, .T. ) ;
#13202 = ORIENTED_EDGE ( 'NONE', *, *, #23624, .T. ) ;
#13203 = VECTOR ( 'NONE', #1841, 1000.000000000000000 ) ;
#13204 = ORIENTED_EDGE ( 'NONE', *, *, #775, .F. ) ;
#13205 = ADVANCED_FACE ( 'NONE', ( #26210 ), #19182, .F. ) ;
#13206 = ORIENTED_EDGE ( 'NONE', *, *, #26141, .F. ) ;
#13207 = ORIENTED_EDGE ( 'NONE', *, *, #26700, .T. ) ;
#13208 = VERTEX_POINT ( 'NONE', #28217 ) ;
#13209 = CARTESIAN_POINT ( 'NONE',  ( -210.0000000000000284, 59.99999999999993605, -70.00000000000001421 ) ) ;
#13210 = DIRECTION ( 'NONE',  ( 0.4528218681377911836, 0.8916010070296023216, -0.000000000000000000 ) ) ;
#13211 = UNCERTAINTY_MEASURE_WITH_UNIT (LENGTH_MEASURE( 1.000000000000000082E-05 ), #10035, 'distance_accuracy_value', 'NONE');
#13212 = FACE_OUTER_BOUND ( 'NONE', #27661, .T. ) ;
#13213 = ADVANCED_FACE ( 'NONE', ( #3951 ), #21478, .F. ) ;
#13214 = CARTESIAN_POINT ( 'NONE',  ( -204.6417490964275885, 60.41478268044740219, 22.13567842568468436 ) ) ;
#13216 = VECTOR ( 'NONE', #20663, 1000.000000000000000 ) ;
#13215 = CYLINDRICAL_SURFACE ( 'NONE', #8734, 30.00000000000000000 ) ;
#13217 = PLANE ( 'NONE',  #3477 ) ;
#13218 = FACE_OUTER_BOUND ( 'NONE', #9341, .T. ) ;
#13219 = CARTESIAN_POINT ( 'NONE',  ( 157.4999999999997442, 253.8563126013445697, 45.00000000000000000 ) ) ;
#13220 = SHAPE_REPRESENTATION ( 'Sliding Carriage', ( #10637 ), #7887 ) ;
#13221 = DIRECTION ( 'NONE',  ( 0.000000000000000000, 0.000000000000000000, -1.000000000000000000 ) ) ;
#13222 = CARTESIAN_POINT ( 'NONE',  ( -224.6648725863131233, 72.14980496866132853, -18.55523389629916409 ) ) ;
#13223 = ADVANCED_FACE ( 'NONE', ( #19326 ), #4374, .F. ) ;
#13224 = LINE ( 'NONE', #19675, #9579 ) ;
#13225 = FACE_OUTER_BOUND ( 'NONE', #11728, .T. ) ;
#13226 = FACE_OUTER_BOUND ( 'NONE', #435, .T. ) ;
#13227 = CARTESIAN_POINT ( 'NONE',  ( 158.0000000000011937, 91.09837461714084839, 45.00000000000000000 ) ) ;
#13229 = VERTEX_POINT ( 'NONE', #17175 ) ;
#13228 = ORIENTED_EDGE ( 'NONE', *, *, #19382, .F. ) ;
#13230 = CARTESIAN_POINT ( 'NONE',  ( -228.3238744270677500, 88.44394938709523046, -15.56515158583171576 ) ) ;
#13231 = AXIS2_PLACEMENT_3D ( 'NONE', #6538, #2079, #2213 ) ;
#13232 = CARTESIAN_POINT ( 'NONE',  ( 157.9999999999998010, 238.5551250525490161, -45.00000000000000000 ) ) ;
#13233 = ORIENTED_EDGE ( 'NONE', *, *, #11972, .T. ) ;
#13234 = VERTEX_POINT ( 'NONE', #12877 ) ;
#13235 = ORIENTED_EDGE ( 'NONE', *, *, #10298, .T. ) ;
#13236 = VECTOR ( 'NONE', #13761, 1000.000000000000000 ) ;
#13237 = ADVANCED_FACE ( 'NONE', ( #21622 ), #19470, .F. ) ;
#13238 = CARTESIAN_POINT ( 'NONE',  ( 79.99999999999991473, 140.0000000000000000, 100.0000000000000142 ) ) ;
#13239 = CARTESIAN_POINT ( 'NONE',  ( 157.4999999999994600, 216.2381874887387880, -45.00000000000000000 ) ) ;
#13240 = VECTOR ( 'NONE', #13576, 999.9999999999998863 ) ;
#13241 = VERTEX_POINT ( 'NONE', #26069 ) ;
#13242 = CARTESIAN_POINT ( 'NONE',  ( 96.92716526682083611, 115.1868982021453149, -77.49999999976235188 ) ) ;
#13243 = DIRECTION ( 'NONE',  ( 1.000000000000000000, 0.000000000000000000, 0.000000000000000000 ) ) ;
#13244 = VERTEX_POINT ( 'NONE', #19611 ) ;
#13245 = CARTESIAN_POINT ( 'NONE',  ( -209.0571706919526775, 89.42610521641519483, 24.27378870941836198 ) ) ;
#13246 = CARTESIAN_POINT ( 'NONE',  ( 134.9999999999998579, 220.0000000000000284, -119.9999999999999858 ) ) ;
#13247 = ADVANCED_FACE ( 'NONE', ( #15174 ), #21771, .F. ) ;
#13248 = VECTOR ( 'NONE', #23777, 1000.000000000000227 ) ;
#13249 = DIRECTION ( 'NONE',  ( -1.000000000000000000, 0.000000000000000000, 0.000000000000000000 ) ) ;
#13250 = CARTESIAN_POINT ( 'NONE',  ( 157.6690878436907610, 200.3501690022571609, -146.9353207969096502 ) ) ;
#13251 = EDGE_CURVE ( 'NONE', #17075, #3368, #8031, .T. ) ;
#13252 = AXIS2_PLACEMENT_3D ( 'NONE', #6805, #4790, #15587 ) ;
#13253 = ORIENTED_EDGE ( 'NONE', *, *, #11410, .F. ) ;
#13254 = DIRECTION ( 'NONE',  ( 1.000000000000000000, 0.000000000000000000, 0.000000000000000000 ) ) ;
#13255 = AXIS2_PLACEMENT_3D ( 'NONE', #25810, #6942, #2628 ) ;
#13256 = EDGE_CURVE ( 'NONE', #2012, #12468, #24071, .T. ) ;
#13257 = CARTESIAN_POINT ( 'NONE',  ( -224.0246150495876805, 134.1142769380900575, -12.98324324887284043 ) ) ;
#13258 = PLANE ( 'NONE',  #28061 ) ;
#13259 = DIRECTION ( 'NONE',  ( -0.000000000000000000, 0.000000000000000000, -1.000000000000000000 ) ) ;
#13260 = VERTEX_POINT ( 'NONE', #21909 ) ;
#13261 = DIRECTION ( 'NONE',  ( 0.8916010070297542001, -0.4528218681374919230, 0.000000000000000000 ) ) ;
#13262 = AXIS2_PLACEMENT_3D ( 'NONE', #22280, #17823, #13243 ) ;
#13263 = LINE ( 'NONE', #37, #7503 ) ;
#13264 = CARTESIAN_POINT ( 'NONE',  ( 203.1730087600953993, 54.44004362106413453, 45.00000000000000000 ) ) ;
#13265 = ORIENTED_EDGE ( 'NONE', *, *, #3753, .T. ) ;
#13266 = ORIENTED_EDGE ( 'NONE', *, *, #10319, .F. ) ;
#13267 = DIRECTION ( 'NONE',  ( -0.000000000000000000, -0.000000000000000000, -1.000000000000000000 ) ) ;
#13268 = AXIS2_PLACEMENT_3D ( 'NONE', #214, #17447, #19743 ) ;
#13269 = CARTESIAN_POINT ( 'NONE',  ( -194.8998556634137174, 99.79200883561803437, -31.71479442048328323 ) ) ;
#13270 = VERTEX_POINT ( 'NONE', #2212 ) ;
#13271 = VERTEX_POINT ( 'NONE', #10998 ) ;
#13272 = CARTESIAN_POINT ( 'NONE',  ( 134.9999999999998579, 220.0000000000000284, 109.9999999999999858 ) ) ;
#13273 = VECTOR ( 'NONE', #9112, 1000.000000000000000 ) ;
#13274 = PRODUCT_DEFINITION_SHAPE ( 'NONE', 'NONE',  #28403 ) ;
#13275 = CARTESIAN_POINT ( 'NONE',  ( 158.0000000000017337, 40.94087446699997912, 45.00000000000000000 ) ) ;
#13276 = ORIENTED_EDGE ( 'NONE', *, *, #27105, .T. ) ;
#13277 = VERTEX_POINT ( 'NONE', #19747 ) ;
#13278 = DIRECTION ( 'NONE',  ( 0.9960550913260672878, 1.086714821493792890E-17, 0.08873699929240054518 ) ) ;
#13279 = VECTOR ( 'NONE', #2130, 1000.000000000000000 ) ;
#13280 = DIRECTION ( 'NONE',  ( 0.6681556583950252204, 0.7440215159218921404, -0.000000000000000000 ) ) ;
#13281 = DIRECTION ( 'NONE',  ( 0.000000000000000000, 0.000000000000000000, -1.000000000000000000 ) ) ;
#13282 = DIRECTION ( 'NONE',  ( 0.9506505318133474658, -0.3102637045530776683, 0.000000000000000000 ) ) ;
#13283 = ADVANCED_FACE ( 'NONE', ( #17592 ), #14745, .F. ) ;
#13284 = DIRECTION ( 'NONE',  ( -0.000000000000000000, 0.000000000000000000, 1.000000000000000000 ) ) ;
#13285 = EDGE_CURVE ( 'NONE', #15999, #15612, #11723, .T. ) ;
#13286 = CARTESIAN_POINT ( 'NONE',  ( 158.0000000000017337, 42.94087446699998623, 45.00000000000000000 ) ) ;
#13287 = CARTESIAN_POINT ( 'NONE',  ( -260.0000000000001137, -157.0000000000000284, -94.99999999999985789 ) ) ;
#13288 = EDGE_LOOP ( 'NONE', ( #21633, #449, #19753, #11181 ) ) ;
#13289 = AXIS2_PLACEMENT_3D ( 'NONE', #6561, #21792, #17615 ) ;
#13290 = CARTESIAN_POINT ( 'NONE',  ( -219.2467648448761395, 139.5102435001769265, 5.000000000000002665 ) ) ;
#13291 = VECTOR ( 'NONE', #27252, 1000.000000000000000 ) ;
#13292 = DIRECTION ( 'NONE',  ( 1.049727191138617586E-16, 0.5150380749100552658, -0.8571673007021115565 ) ) ;
#13293 = CARTESIAN_POINT ( 'NONE',  ( 154.4185842870419663, 232.3660254037841639, 45.00000000000000000 ) ) ;
#13294 = DIRECTION ( 'NONE',  ( -0.000000000000000000, -0.000000000000000000, -1.000000000000000000 ) ) ;
#13295 = ORIENTED_EDGE ( 'NONE', *, *, #10407, .F. ) ;
#13296 = DIRECTION ( 'NONE',  ( -0.8916010070295106171, 0.4528218681379715393, 0.000000000000000000 ) ) ;
#13297 = AXIS2_PLACEMENT_3D ( 'NONE', #17660, #17799, #26555 ) ;
#13298 = ORIENTED_EDGE ( 'NONE', *, *, #16939, .F. ) ;
#13299 = CYLINDRICAL_SURFACE ( 'NONE', #15732, 22.49999999999999289 ) ;
#13300 = CARTESIAN_POINT ( 'NONE',  ( 136.9323230404753815, 249.9383011342688974, -150.6837522856750411 ) ) ;
#13301 = ORIENTED_EDGE ( 'NONE', *, *, #10312, .T. ) ;
#13302 = CARTESIAN_POINT ( 'NONE',  ( 22.58950924271104554, 154.2349915562422780, -13.00000000000000000 ) ) ;
#13303 = ORIENTED_EDGE ( 'NONE', *, *, #9960, .T. ) ;
#13304 = CIRCLE ( 'NONE', #27322, 22.49999999999997868 ) ;
#13305 = CARTESIAN_POINT ( 'NONE',  ( 157.4999999999998579, 183.6358123911478799, -45.00000000000000000 ) ) ;
#13306 = ORIENTED_EDGE ( 'NONE', *, *, #376, .F. ) ;
#13307 = EDGE_CURVE ( 'NONE', #1799, #7680, #2517, .T. ) ;
#13308 = EDGE_LOOP ( 'NONE', ( #6645, #7881, #27700, #10920 ) ) ;
#13309 = ORIENTED_EDGE ( 'NONE', *, *, #27725, .F. ) ;
#13310 = CARTESIAN_POINT ( 'NONE',  ( 158.0000000000010516, 105.6377496546760568, 45.00000000000000000 ) ) ;
#13311 = CIRCLE ( 'NONE', #24794, 43.76444293738737912 ) ;
#13312 = ADVANCED_FACE ( 'NONE', ( #20466 ), #7109, .T. ) ;
#13313 = VERTEX_POINT ( 'NONE', #15744 ) ;
#13314 = VERTEX_POINT ( 'NONE', #19892 ) ;
#13315 = CARTESIAN_POINT ( 'NONE',  ( -226.9034654753193365, 131.5715075452304745, 15.04814241295084543 ) ) ;
#13316 = CARTESIAN_POINT ( 'NONE',  ( 94.58250724493628070, 231.5191281348353982, 18.77838886173626420 ) ) ;
#13317 = TOROIDAL_SURFACE ( 'NONE', #4559, 20.00000000000000355, 30.00000000000000000 ) ;
#13318 = DIRECTION ( 'NONE',  ( 0.8660254037844359321, -0.5000000000000045519, 0.000000000000000000 ) ) ;
#13319 = ADVANCED_FACE ( 'NONE', ( #20031 ), #26350, .F. ) ;
#13320 = FACE_OUTER_BOUND ( 'NONE', #22558, .T. ) ;
#13321 = EDGE_CURVE ( 'NONE', #10473, #7097, #8979, .T. ) ;
#13322 = CARTESIAN_POINT ( 'NONE',  ( 158.7404207507997853, 42.53436754635193040, -45.00000000000000000 ) ) ;
#13323 = DIRECTION ( 'NONE',  ( -0.000000000000000000, -0.000000000000000000, 1.000000000000000000 ) ) ;
#13324 = PLANE ( 'NONE',  #17538 ) ;
#13325 = EDGE_CURVE ( 'NONE', #20275, #2290, #24561, .T. ) ;
#13326 = CARTESIAN_POINT ( 'NONE',  ( -160.0000000000000284, 109.9999999999999432, 100.0000000000000142 ) ) ;
#13327 = FACE_OUTER_BOUND ( 'NONE', #20596, .T. ) ;
#13328 = DIRECTION ( 'NONE',  ( 0.4528218681383106015, -0.8916010070293384215, 0.000000000000000000 ) ) ;
#13329 = FACE_BOUND ( 'NONE', #23056, .T. ) ;
#13330 = CARTESIAN_POINT ( 'NONE',  ( 197.6424708188942816, 64.50455043276784295, 45.00000000000000000 ) ) ;
#13331 = ORIENTED_EDGE ( 'NONE', *, *, #7195, .T. ) ;
#13332 = DIRECTION ( 'NONE',  ( 0.000000000000000000, 0.000000000000000000, 1.000000000000000000 ) ) ;
#13333 = VECTOR ( 'NONE', #11882, 1000.000000000000000 ) ;
#13334 = DIRECTION ( 'NONE',  ( 0.8916010070293383105, -0.4528218681383106015, 0.000000000000000000 ) ) ;
#13335 = LINE ( 'NONE', #15492, #17643 ) ;
#13336 = CYLINDRICAL_SURFACE ( 'NONE', #4659, 5.999999999999991118 ) ;
#13337 = ORIENTED_EDGE ( 'NONE', *, *, #3451, .T. ) ;
#13338 = VECTOR ( 'NONE', #10533, 1000.000000000000000 ) ;
#13339 = APPLICATION_CONTEXT ( 'automotive_design' ) ;
#13340 = LINE ( 'NONE', #13630, #23973 ) ;
#13341 = ORIENTED_EDGE ( 'NONE', *, *, #5359, .F. ) ;
#13342 = CARTESIAN_POINT ( 'NONE',  ( 8.117852850209610338, 141.5785587194356197, -13.00000000000000000 ) ) ;
#13343 = ORIENTED_EDGE ( 'NONE', *, *, #13064, .F. ) ;
#13344 = ORIENTED_EDGE ( 'NONE', *, *, #14074, .T. ) ;
#13345 = EDGE_LOOP ( 'NONE', ( #23399, #1173, #23543, #17391 ) ) ;
#13346 = ORIENTED_EDGE ( 'NONE', *, *, #15432, .T. ) ;
#13347 = DIRECTION ( 'NONE',  ( 0.000000000000000000, 0.000000000000000000, -1.000000000000000000 ) ) ;
#13348 = DIRECTION ( 'NONE',  ( 0.8916010070296732648, 0.4528218681376511845, 0.000000000000000000 ) ) ;
#13349 = EDGE_CURVE ( 'NONE', #28280, #26741, #5340, .T. ) ;
#13350 = EDGE_CURVE ( 'NONE', #4902, #27901, #14431, .T. ) ;
#13351 = VECTOR ( 'NONE', #20524, 1000.000000000000227 ) ;
#13352 = FACE_OUTER_BOUND ( 'NONE', #24417, .T. ) ;
#13353 = PLANE ( 'NONE',  #13974 ) ;
#13354 = VECTOR ( 'NONE', #1196, 1000.000000000000000 ) ;
#13355 = CARTESIAN_POINT ( 'NONE',  ( -202.1528982378584658, 60.83080389531669852, 24.93098023360008142 ) ) ;
#13356 = LINE ( 'NONE', #24838, #22609 ) ;
#13357 = CARTESIAN_POINT ( 'NONE',  ( 158.0000000000001137, 193.9212499249295831, 45.00000000000000000 ) ) ;
#13358 = EDGE_CURVE ( 'NONE', #27297, #16487, #14568, .T. ) ;
#13359 = DIRECTION ( 'NONE',  ( -1.000000000000000000, -2.602085213965211135E-16, 0.000000000000000000 ) ) ;
#13360 = CARTESIAN_POINT ( 'NONE',  ( -40.40953891503691153, 0.000000000000000000, 99.00000000000000000 ) ) ;
#13361 = FACE_OUTER_BOUND ( 'NONE', #3523, .T. ) ;
#13362 = CARTESIAN_POINT ( 'NONE',  ( 88.58553289623721128, 111.2425746091579413, 71.46484375014649970 ) ) ;
#13363 = EDGE_CURVE ( 'NONE', #11039, #22451, #1067, .T. ) ;
#13364 = CARTESIAN_POINT ( 'NONE',  ( -5.148328491344469349, 133.7892143339873599, 15.61121058808317841 ) ) ;
#13365 = CARTESIAN_POINT ( 'NONE',  ( -210.0000000000000284, 59.99999999999994316, 17.29233506344265336 ) ) ;
#13366 = DIRECTION ( 'NONE',  ( -0.8916010070297345491, -0.4528218681375307253, 0.000000000000000000 ) ) ;
#13367 = CARTESIAN_POINT ( 'NONE',  ( 157.4999999999998579, 153.5413123010633853, -45.00000000000000000 ) ) ;
#13369 = ORIENTED_EDGE ( 'NONE', *, *, #19674, .T. ) ;
#13368 = EDGE_LOOP ( 'NONE', ( #24336, #5132, #13703, #15566 ) ) ;
#13370 = CARTESIAN_POINT ( 'NONE',  ( -181.6419045364029614, 108.9881197006330353, 30.31385955260705956 ) ) ;
#13371 = VECTOR ( 'NONE', #17263, 1000.000000000000000 ) ;
#13372 = CARTESIAN_POINT ( 'NONE',  ( 157.4999999999998579, 73.28931206083800021, 45.00000000000000000 ) ) ;
#13373 = ORIENTED_EDGE ( 'NONE', *, *, #1822, .T. ) ;
#13374 = ORIENTED_EDGE ( 'NONE', *, *, #27412, .F. ) ;
#13375 = EDGE_LOOP ( 'NONE', ( #3742, #25099, #10437, #18943 ) ) ;
#13376 = AXIS2_PLACEMENT_3D ( 'NONE', #19814, #17800, #13507 ) ;
#13377 = DIRECTION ( 'NONE',  ( 0.000000000000000000, -1.000000000000000000, 0.000000000000000000 ) ) ;
#13378 = CARTESIAN_POINT ( 'NONE',  ( -97.83317650214073069, 134.5241583270075978, 15.50066840981723182 ) ) ;
#13379 = ORIENTED_EDGE ( 'NONE', *, *, #17090, .F. ) ;
#13380 = CARTESIAN_POINT ( 'NONE',  ( -196.7918453702777128, 71.54464929955099706, 82.80879831960034210 ) ) ;
#13381 = EDGE_CURVE ( 'NONE', #8519, #14427, #11727, .T. ) ;
#13382 = EDGE_CURVE ( 'NONE', #1139, #749, #1205, .T. ) ;
#13383 = LINE ( 'NONE', #22134, #10976 ) ;
#13384 = ORIENTED_EDGE ( 'NONE', *, *, #24504, .F. ) ;
#13385 = CARTESIAN_POINT ( 'NONE',  ( -209.0251556266169075, 89.43021808311971199, 25.51491776097941511 ) ) ;
#13386 = CARTESIAN_POINT ( 'NONE',  ( -212.5524510162168212, -218.0941723687617184, 106.4974602408248074 ) ) ;
#13387 = VECTOR ( 'NONE', #8268, 1000.000000000000114 ) ;
#13388 = DIRECTION ( 'NONE',  ( -0.000000000000000000, 0.000000000000000000, -1.000000000000000000 ) ) ;
#13389 = AXIS2_PLACEMENT_3D ( 'NONE', #5900, #1591, #14674 ) ;
#13390 = CARTESIAN_POINT ( 'NONE',  ( 157.5598940431783603, 200.2249467617852190, -146.3660979730027520 ) ) ;
#13391 = VECTOR ( 'NONE', #6738, 1000.000000000000000 ) ;
#13392 = EDGE_LOOP ( 'NONE', ( #1901, #14160, #11961, #7074, #1632, #28001, #1984, #14091 ) ) ;
#13393 = ADVANCED_FACE ( 'NONE', ( #9970 ), #9421, .T. ) ;
#13394 = ADVANCED_FACE ( 'NONE', ( #1346 ), #23634, .T. ) ;
#13395 = DIRECTION ( 'NONE',  ( 1.000000000000000000, -0.000000000000000000, -0.000000000000000000 ) ) ;
#13396 = CARTESIAN_POINT ( 'NONE',  ( 146.9844428835009467, 225.6878133005969858, 45.00000000000000000 ) ) ;
#13397 = DIRECTION ( 'NONE',  ( 1.000000000000000000, 0.000000000000000000, -1.921731041659628380E-16 ) ) ;
#13398 = FACE_OUTER_BOUND ( 'NONE', #26529, .T. ) ;
#13399 = ORIENTED_EDGE ( 'NONE', *, *, #8741, .T. ) ;
#13400 = CARTESIAN_POINT ( 'NONE',  ( -210.0000000000000568, -220.0000000000000853, -109.1217062362807155 ) ) ;
#13401 = CARTESIAN_POINT ( 'NONE',  ( 157.4999999999997158, 263.8878126313725829, -45.00000000000000000 ) ) ;
#13402 = DIRECTION ( 'NONE',  ( 0.8916010070296429557, -0.4528218681377111920, 0.000000000000000000 ) ) ;
#13403 = ORIENTED_EDGE ( 'NONE', *, *, #21709, .F. ) ;
#13404 = ORIENTED_EDGE ( 'NONE', *, *, #6181, .F. ) ;
#13405 = EDGE_CURVE ( 'NONE', #8289, #5518, #25193, .T. ) ;
#13406 = EDGE_CURVE ( 'NONE', #17461, #16305, #22770, .T. ) ;
#13407 = VECTOR ( 'NONE', #9963, 1000.000000000000227 ) ;
#13408 = DIRECTION ( 'NONE',  ( -0.000000000000000000, -0.000000000000000000, -1.000000000000000000 ) ) ;
#13409 = LINE ( 'NONE', #13701, #26403 ) ;
#13410 = ORIENTED_EDGE ( 'NONE', *, *, #21318, .F. ) ;
#13411 = LINE ( 'NONE', #2131, #19444 ) ;
#13412 = ORIENTED_EDGE ( 'NONE', *, *, #5748, .F. ) ;
#13413 = PLANE ( 'NONE',  #18666 ) ;
#13414 = DIRECTION ( 'NONE',  ( 0.000000000000000000, 0.000000000000000000, -1.000000000000000000 ) ) ;
#13415 = ORIENTED_EDGE ( 'NONE', *, *, #17947, .T. ) ;
#13416 = ORIENTED_EDGE ( 'NONE', *, *, #20319, .F. ) ;
#13417 = DIRECTION ( 'NONE',  ( -0.000000000000000000, 0.000000000000000000, 1.000000000000000000 ) ) ;
#13418 = CARTESIAN_POINT ( 'NONE',  ( 158.0000000000009663, 113.1613746771971876, -45.00000000000000000 ) ) ;
#13419 = DIRECTION ( 'NONE',  ( -0.000000000000000000, -0.000000000000000000, -1.000000000000000000 ) ) ;
#13420 = FACE_OUTER_BOUND ( 'NONE', #17749, .T. ) ;
#13421 = CARTESIAN_POINT ( 'NONE',  ( 158.0000000000009095, 118.6849996997183041, 45.00000000000000000 ) ) ;
#13422 = VECTOR ( 'NONE', #17046, 1000.000000000000000 ) ;
#13423 = DIRECTION ( 'NONE',  ( -0.000000000000000000, -0.000000000000000000, -1.000000000000000000 ) ) ;
#13424 = CARTESIAN_POINT ( 'NONE',  ( 367.4999999999996021, -5.589247009368149222, 1.243177022048955014E-14 ) ) ;
#13425 = VERTEX_POINT ( 'NONE', #7400 ) ;
#13426 = EDGE_CURVE ( 'NONE', #13994, #12360, #5514, .T. ) ;
#13427 = VECTOR ( 'NONE', #18410, 1000.000000000000000 ) ;
#13428 = CARTESIAN_POINT ( 'NONE',  ( 157.9999999999998010, 234.0472500450420341, -45.00000000000000000 ) ) ;
#13429 = DIRECTION ( 'NONE',  ( 1.000000000000000000, 8.673617379884036705E-17, 0.000000000000000000 ) ) ;
#13431 = PLANE ( 'NONE',  #6819 ) ;
#13430 = VECTOR ( 'NONE', #23560, 1000.000000000000227 ) ;
#13432 = DIRECTION ( 'NONE',  ( -0.000000000000000000, -0.000000000000000000, -1.000000000000000000 ) ) ;
#13433 = VERTEX_POINT ( 'NONE', #3354 ) ;
#13434 = DIRECTION ( 'NONE',  ( 4.625929269271489858E-16, -0.000000000000000000, 1.000000000000000000 ) ) ;
#13435 = VECTOR ( 'NONE', #16726, 1000.000000000000000 ) ;
#13436 = EDGE_LOOP ( 'NONE', ( #10253, #24352, #22090, #23154 ) ) ;
#13437 = FACE_OUTER_BOUND ( 'NONE', #26973, .T. ) ;
#13438 = DIRECTION ( 'NONE',  ( -1.000000000000000000, 0.000000000000000000, 0.000000000000000000 ) ) ;
#13439 = CARTESIAN_POINT ( 'NONE',  ( 140.3919500952845283, 249.5118635391362716, -147.6607294899351075 ) ) ;
#13440 = VERTEX_POINT ( 'NONE', #18730 ) ;
#13441 = DIRECTION ( 'NONE',  ( 0.8916010070297037959, -0.4528218681375912325, 0.000000000000000000 ) ) ;
#13442 = VERTEX_POINT ( 'NONE', #12144 ) ;
#13443 = CARTESIAN_POINT ( 'NONE',  ( -208.6642397829361926, 74.78008005802638536, 37.85499228847417186 ) ) ;
#13444 = EDGE_LOOP ( 'NONE', ( #9278, #3219, #14527, #21736 ) ) ;
#13445 = CARTESIAN_POINT ( 'NONE',  ( -272.7817474293340183, -170.1432013118196380, 92.71875118442027031 ) ) ;
#13446 = ORIENTED_EDGE ( 'NONE', *, *, #24177, .F. ) ;
#13447 = ADVANCED_FACE ( 'NONE', ( #16308 ), #4347, .F. ) ;
#13448 = AXIS2_PLACEMENT_3D ( 'NONE', #24471, #7089, #22170 ) ;
#13449 = VERTEX_POINT ( 'NONE', #7956 ) ;
#13450 = EDGE_CURVE ( 'NONE', #21245, #5808, #7543, .T. ) ;
#13451 = DIRECTION ( 'NONE',  ( 0.8916010070293584056, -0.4528218681382712996, 0.000000000000000000 ) ) ;
#13452 = ORIENTED_EDGE ( 'NONE', *, *, #28271, .T. ) ;
#13453 = CIRCLE ( 'NONE', #16209, 7.999999999999979572 ) ;
#13454 = EDGE_CURVE ( 'NONE', #19970, #17350, #12425, .T. ) ;
#13455 = ORIENTED_EDGE ( 'NONE', *, *, #2679, .T. ) ;
#13456 = VERTEX_POINT ( 'NONE', #18317 ) ;
#13457 = VECTOR ( 'NONE', #14522, 1000.000000000000000 ) ;
#13458 = CARTESIAN_POINT ( 'NONE',  ( 99.07849735471529584, 234.2556710009807546, 21.83147064533734394 ) ) ;
#13459 = AXIS2_PLACEMENT_3D ( 'NONE', #9700, #18461, #5241 ) ;
#13460 = LINE ( 'NONE', #22069, #3866 ) ;
#13461 = CARTESIAN_POINT ( 'NONE',  ( -213.1827219047386848, -216.7767438708612531, 105.0000000000000142 ) ) ;
#13462 = CARTESIAN_POINT ( 'NONE',  ( 157.9999999999997442, 256.1102501050980322, 45.00000000000000000 ) ) ;
#13463 = CARTESIAN_POINT ( 'NONE',  ( -272.4467628956543876, -165.0365710123801648, 87.32694055142955847 ) ) ;
#13464 = CYLINDRICAL_SURFACE ( 'NONE', #18919, 30.00000000000000000 ) ;
#13465 = DIRECTION ( 'NONE',  ( 0.000000000000000000, 0.000000000000000000, -1.000000000000000000 ) ) ;
#13466 = DIRECTION ( 'NONE',  ( -1.000000000000000000, 0.000000000000000000, 0.000000000000000000 ) ) ;
#13467 = CARTESIAN_POINT ( 'NONE',  ( 217.4999999999996305, -5.589247009368136787, -100.0000000000000142 ) ) ;
#13468 = DIRECTION ( 'NONE',  ( 0.000000000000000000, -1.000000000000000000, -1.214306433183764966E-16 ) ) ;
#13469 = CARTESIAN_POINT ( 'NONE',  ( 157.4999999999998579, 156.0491873085704242, -45.00000000000000000 ) ) ;
#13470 = ORIENTED_EDGE ( 'NONE', *, *, #19791, .F. ) ;
#13471 = VECTOR ( 'NONE', #8075, 1000.000000000000000 ) ;
#13472 = CARTESIAN_POINT ( 'NONE',  ( 158.0000000000009095, 120.6849996997183183, 45.00000000000000000 ) ) ;
#13473 = VECTOR ( 'NONE', #16443, 999.9999999999998863 ) ;
#13474 = DIRECTION ( 'NONE',  ( 0.000000000000000000, 0.000000000000000000, -1.000000000000000000 ) ) ;
#13475 = CARTESIAN_POINT ( 'NONE',  ( 124.3660254037845192, 199.5814157129575506, -45.00000000000000000 ) ) ;
#13476 = DIRECTION ( 'NONE',  ( 0.000000000000000000, 0.000000000000000000, 1.000000000000000000 ) ) ;
#13477 = ORIENTED_EDGE ( 'NONE', *, *, #8287, .F. ) ;
#13478 = DIRECTION ( 'NONE',  ( 0.8916010070296935819, 0.4528218681376112165, 0.000000000000000000 ) ) ;
#13479 = VERTEX_POINT ( 'NONE', #14153 ) ;
#13480 = LINE ( 'NONE', #6439, #4483 ) ;
#13481 = VERTEX_POINT ( 'NONE', #16582 ) ;
#13482 = ADVANCED_FACE ( 'NONE', ( #27067 ), #25337, .T. ) ;
#13483 = ORIENTED_EDGE ( 'NONE', *, *, #900, .F. ) ;
#13484 = EDGE_CURVE ( 'NONE', #18244, #2835, #24168, .T. ) ;
#13485 = EDGE_CURVE ( 'NONE', #24950, #19061, #12705, .T. ) ;
#13486 = EDGE_CURVE ( 'NONE', #999, #16719, #14026, .T. ) ;
#13487 = ORIENTED_EDGE ( 'NONE', *, *, #23656, .F. ) ;
#13488 = ORIENTED_EDGE ( 'NONE', *, *, #13540, .F. ) ;
#13489 = ORIENTED_EDGE ( 'NONE', *, *, #758, .T. ) ;
#13490 = LINE ( 'NONE', #22678, #8128 ) ;
#13491 = CIRCLE ( 'NONE', #9369, 1.000000000000000888 ) ;
#13492 = DIRECTION ( 'NONE',  ( -1.000000000000000000, 0.000000000000000000, 0.000000000000000000 ) ) ;
#13493 = LINE ( 'NONE', #20082, #12065 ) ;
#13494 = PLANE ( 'NONE',  #6871 ) ;
#13495 = AXIS2_PLACEMENT_3D ( 'NONE', #2782, #645, #9259 ) ;
#13496 = CARTESIAN_POINT ( 'NONE',  ( 157.4999999999996589, 278.9350626764145318, 45.00000000000000000 ) ) ;
#13497 = CARTESIAN_POINT ( 'NONE',  ( -216.3288264717405696, 60.34946693787963312, 12.99564918865531382 ) ) ;
#13498 = DIRECTION ( 'NONE',  ( 0.000000000000000000, 0.000000000000000000, -1.000000000000000000 ) ) ;
#13499 = CARTESIAN_POINT ( 'NONE',  ( 33.10302365956999182, 203.2034914284457159, 12.99999999999999822 ) ) ;
#13500 = CARTESIAN_POINT ( 'NONE',  ( 157.9999999999997726, 246.5866250825770294, -45.00000000000000000 ) ) ;
#13501 = DIRECTION ( 'NONE',  ( -0.8916010070293584056, -0.4528218681382712996, 0.000000000000000000 ) ) ;
#13502 = CARTESIAN_POINT ( 'NONE',  ( 158.0000000000013358, 78.55899957960562574, 45.00000000000000000 ) ) ;
#13503 = DIRECTION ( 'NONE',  ( 0.4528218681374719945, 0.8916010070297644141, -0.000000000000000000 ) ) ;
#13504 = DIRECTION ( 'NONE',  ( 0.8916010070295715684, -0.4528218681378516353, 0.000000000000000000 ) ) ;
#13505 = LINE ( 'NONE', #7178, #6360 ) ;
#13506 = CARTESIAN_POINT ( 'NONE',  ( -209.1829431684195129, 69.04425972296263581, 36.49229859027995815 ) ) ;
#13507 = DIRECTION ( 'NONE',  ( 0.000000000000000000, 0.000000000000000000, -1.000000000000000000 ) ) ;
#13508 = DIRECTION ( 'NONE',  ( -0.000000000000000000, -0.000000000000000000, -1.000000000000000000 ) ) ;
#13510 = ORIENTED_EDGE ( 'NONE', *, *, #24935, .F. ) ;
#13509 = ORIENTED_EDGE ( 'NONE', *, *, #22707, .T. ) ;
#13511 = AXIS2_PLACEMENT_3D ( 'NONE', #19278, #6763, #24441 ) ;
#13512 = CARTESIAN_POINT ( 'NONE',  ( 157.9999999999996589, 274.1732501651540588, -45.00000000000000000 ) ) ;
#13513 = EDGE_CURVE ( 'NONE', #5554, #28289, #1603, .T. ) ;
#13514 = EDGE_CURVE ( 'NONE', #212, #18655, #17663, .T. ) ;
#13515 = CARTESIAN_POINT ( 'NONE',  ( 125.3433571860710884, 197.9412384757604286, 0.000000000000000000 ) ) ;
#13516 = CARTESIAN_POINT ( 'NONE',  ( -207.8525085575914488, 89.95873525663041903, -26.39520176074849545 ) ) ;
#13517 = ORIENTED_EDGE ( 'NONE', *, *, #8300, .T. ) ;
#13518 = AXIS2_PLACEMENT_3D ( 'NONE', #21580, #15129, #27751 ) ;
#13519 = ORIENTED_EDGE ( 'NONE', *, *, #11663, .F. ) ;
#13520 = VERTEX_POINT ( 'NONE', #10394 ) ;
#13521 = EDGE_CURVE ( 'NONE', #24416, #7370, #21331, .T. ) ;
#13522 = DIRECTION ( 'NONE',  ( -1.000000000000000000, 0.000000000000000000, 0.000000000000000000 ) ) ;
#13523 = CARTESIAN_POINT ( 'NONE',  ( -144.6612699377151046, 126.7250878843629778, 18.05549492154933233 ) ) ;
#13524 = EDGE_CURVE ( 'NONE', #12071, #15387, #10677, .T. ) ;
#13525 = VERTEX_POINT ( 'NONE', #27894 ) ;
#13526 = ORIENTED_EDGE ( 'NONE', *, *, #2985, .T. ) ;
#13527 = CARTESIAN_POINT ( 'NONE',  ( 9.999999999999957367, -20.00000000000004974, 110.0000000000000284 ) ) ;
#13528 = VECTOR ( 'NONE', #18115, 1000.000000000000000 ) ;
#13529 = FACE_OUTER_BOUND ( 'NONE', #11259, .T. ) ;
#13530 = VERTEX_POINT ( 'NONE', #6077 ) ;
#13531 = CARTESIAN_POINT ( 'NONE',  ( 145.6339745962154097, 240.4185842870418242, -45.00000000000000000 ) ) ;
#13532 = VECTOR ( 'NONE', #20586, 1000.000000000000000 ) ;
#13533 = CARTESIAN_POINT ( 'NONE',  ( -212.8298628423295895, -217.6190342207067374, 105.9424056457623777 ) ) ;
#13534 = DIRECTION ( 'NONE',  ( -0.000000000000000000, -0.000000000000000000, -1.000000000000000000 ) ) ;
#13535 = AXIS2_PLACEMENT_3D ( 'NONE', #23642, #6395, #10570 ) ;
#13536 = CARTESIAN_POINT ( 'NONE',  ( -160.0000000000000568, 139.9999999999999716, 45.00000000000000000 ) ) ;
#13537 = CARTESIAN_POINT ( 'NONE',  ( -214.6111699653790197, 58.62522005598040664, -31.77808924747014885 ) ) ;
#13538 = ORIENTED_EDGE ( 'NONE', *, *, #6908, .F. ) ;
#13539 = CARTESIAN_POINT ( 'NONE',  ( 158.0000000000000568, 201.4448749474510407, 45.00000000000000000 ) ) ;
#13540 = EDGE_CURVE ( 'NONE', #18881, #7534, #8950, .T. ) ;
#13541 = CARTESIAN_POINT ( 'NONE',  ( 232.4999999999996305, 83.06687458711267880, -36.86484227207694175 ) ) ;
#13542 = FACE_OUTER_BOUND ( 'NONE', #8704, .T. ) ;
#13543 = CARTESIAN_POINT ( 'NONE',  ( 222.4999999999996021, 194.4107529906318064, 58.31593845887894645 ) ) ;
#13544 = ORIENTED_EDGE ( 'NONE', *, *, #14366, .F. ) ;
#13545 = PLANE ( 'NONE',  #23388 ) ;
#13546 = EDGE_CURVE ( 'NONE', #19895, #12172, #13129, .T. ) ;
#13547 = CARTESIAN_POINT ( 'NONE',  ( 157.4999999999998579, 220.0000000000000284, -90.00000000000002842 ) ) ;
#13548 = CARTESIAN_POINT ( 'NONE',  ( 199.9999999999997726, -160.0000000000001990, -110.0000000000000284 ) ) ;
#13549 = ORIENTED_EDGE ( 'NONE', *, *, #6690, .F. ) ;
#13550 =( NAMED_UNIT ( * ) PLANE_ANGLE_UNIT ( ) SI_UNIT ( $, .RADIAN. ) );
#13551 = ORIENTED_EDGE ( 'NONE', *, *, #11461, .F. ) ;
#13552 = CONICAL_SURFACE ( 'NONE', #27286, 30.00000000000001421, 0.7853981633974500554 ) ;
#13553 = CARTESIAN_POINT ( 'NONE',  ( 158.0000000000010516, 105.6377496546760568, 45.00000000000000000 ) ) ;
#13554 = CARTESIAN_POINT ( 'NONE',  ( -200.0107575506397097, 95.40263130992853746, -31.09616731377015597 ) ) ;
#13555 = EDGE_CURVE ( 'NONE', #15494, #18153, #19434, .T. ) ;
#13556 = ORIENTED_EDGE ( 'NONE', *, *, #3339, .F. ) ;
#13557 = AXIS2_PLACEMENT_3D ( 'NONE', #17991, #15852, #2180 ) ;
#13558 = EDGE_LOOP ( 'NONE', ( #11005, #8112, #4467, #7781 ) ) ;
#13559 = DIRECTION ( 'NONE',  ( 0.4528218681373520904, 0.8916010070298252543, -0.000000000000000000 ) ) ;
#13560 = ADVANCED_FACE ( 'NONE', ( #24035 ), #21872, .F. ) ;
#13561 = CARTESIAN_POINT ( 'NONE',  ( 158.0000000000006253, 146.2716247822957598, 45.00000000000000000 ) ) ;
#13562 = ORIENTED_EDGE ( 'NONE', *, *, #20723, .T. ) ;
#13563 = DIRECTION ( 'NONE',  ( 0.8916010070297953893, 0.4528218681374108212, 0.000000000000000000 ) ) ;
#13564 = ORIENTED_EDGE ( 'NONE', *, *, #28331, .F. ) ;
#13565 = CARTESIAN_POINT ( 'NONE',  ( 157.4999999999998579, 103.3838121509225090, -45.00000000000000000 ) ) ;
#13566 = DIRECTION ( 'NONE',  ( 0.000000000000000000, 0.000000000000000000, -1.000000000000000000 ) ) ;
#13567 = AXIS2_PLACEMENT_3D ( 'NONE', #28334, #20012, #4074 ) ;
#13568 = CARTESIAN_POINT ( 'NONE',  ( 157.4999999999998579, 171.0964373536126573, 45.00000000000000000 ) ) ;
#13569 = CARTESIAN_POINT ( 'NONE',  ( -25.38497998821648594, 129.2235485674940776, -16.97173567987970344 ) ) ;
#13570 = DIRECTION ( 'NONE',  ( 1.000000000000000000, -0.000000000000000000, -0.000000000000000000 ) ) ;
#13571 = TOROIDAL_SURFACE ( 'NONE', #1617, 23.59849023212046859, 2.000000000000000000 ) ;
#13572 = EDGE_CURVE ( 'NONE', #24273, #26495, #22497, .T. ) ;
#13573 = CARTESIAN_POINT ( 'NONE',  ( -207.7939942406169109, 74.68924146014083476, -43.59008735158577963 ) ) ;
#13574 = LINE ( 'NONE', #19457, #12363 ) ;
#13575 = EDGE_LOOP ( 'NONE', ( #27490, #5049, #19158, #15573 ) ) ;
#13576 = DIRECTION ( 'NONE',  ( -0.3102637045530707294, -0.9506505318133497973, 0.000000000000000000 ) ) ;
#13577 = VECTOR ( 'NONE', #22730, 1000.000000000000000 ) ;
#13578 = CARTESIAN_POINT ( 'NONE',  ( 122.6339745962156229, 200.5814157129576074, -45.00000000000000000 ) ) ;
#13579 = CARTESIAN_POINT ( 'NONE',  ( 154.8288972274760908, 217.3894761555990556, -45.00000000000000000 ) ) ;
#13580 = CARTESIAN_POINT ( 'NONE',  ( -214.3828916364065833, 175.2783111443768576, -15.00000000000000000 ) ) ;
#13581 = ORIENTED_EDGE ( 'NONE', *, *, #2890, .F. ) ;
#13582 = DIRECTION ( 'NONE',  ( -0.8916010070296531698, -0.4528218681376911525, 0.000000000000000000 ) ) ;
#13583 = ORIENTED_EDGE ( 'NONE', *, *, #4448, .F. ) ;
#13584 = EDGE_CURVE ( 'NONE', #10866, #14018, #25921, .T. ) ;
#13585 = LINE ( 'NONE', #11135, #18515 ) ;
#13586 = CARTESIAN_POINT ( 'NONE',  ( -211.3876077005475906, 59.97725620786449952, -16.20275295307625640 ) ) ;
#13587 = CARTESIAN_POINT ( 'NONE',  ( 138.9634206111875301, 249.7383700032220304, -140.4781857268138765 ) ) ;
#13588 = ORIENTED_EDGE ( 'NONE', *, *, #21347, .T. ) ;
#13589 = LINE ( 'NONE', #20468, #8785 ) ;
#13590 = VERTEX_POINT ( 'NONE', #13548 ) ;
#13591 = CARTESIAN_POINT ( 'NONE',  ( -218.7894661267191054, 71.27542015156993216, 22.74148974320709016 ) ) ;
#13592 = ORIENTED_EDGE ( 'NONE', *, *, #23175, .T. ) ;
#13593 = FACE_OUTER_BOUND ( 'NONE', #22205, .T. ) ;
#13594 = VERTEX_POINT ( 'NONE', #2752 ) ;
#13595 = CIRCLE ( 'NONE', #15899, 50.00000000000000000 ) ;
#13596 = AXIS2_PLACEMENT_3D ( 'NONE', #11157, #241, #9142 ) ;
#13597 = VECTOR ( 'NONE', #17892, 1000.000000000000000 ) ;
#13598 = ORIENTED_EDGE ( 'NONE', *, *, #7195, .F. ) ;
#13599 = EDGE_CURVE ( 'NONE', #6186, #26306, #17556, .T. ) ;
#13600 = DIRECTION ( 'NONE',  ( -1.387778780781444256E-14, -1.000000000000000000, 0.000000000000000000 ) ) ;
#13601 = ORIENTED_EDGE ( 'NONE', *, *, #7515, .T. ) ;
#13602 = EDGE_CURVE ( 'NONE', #12452, #10355, #1154, .T. ) ;
#13603 = VERTEX_POINT ( 'NONE', #4764 ) ;
#13604 = AXIS2_PLACEMENT_3D ( 'NONE', #9478, #18374, #5574 ) ;
#13605 = ORIENTED_EDGE ( 'NONE', *, *, #3401, .T. ) ;
#13606 = CARTESIAN_POINT ( 'NONE',  ( 104.2862437451156268, 245.6633304404780347, 27.19020029358115309 ) ) ;
#13607 = CARTESIAN_POINT ( 'NONE',  ( 95.82124051657368113, -20.23615780638419182, -45.00000000000000000 ) ) ;
#13608 = DIRECTION ( 'NONE',  ( -0.000000000000000000, -0.000000000000000000, -1.000000000000000000 ) ) ;
#13609 = EDGE_CURVE ( 'NONE', #14062, #152, #22442, .T. ) ;
#13610 = CYLINDRICAL_SURFACE ( 'NONE', #10552, 22.49999999999999289 ) ;
#13611 = LINE ( 'NONE', #24365, #12186 ) ;
#13612 = CARTESIAN_POINT ( 'NONE',  ( -79.00187704905530950, 96.44595867864546790, -145.0000000000000000 ) ) ;
#13613 = DIRECTION ( 'NONE',  ( 0.000000000000000000, 0.000000000000000000, 1.000000000000000000 ) ) ;
#13614 = CARTESIAN_POINT ( 'NONE',  ( 134.9999999999998579, 467.1080826427131001, -145.0000000000000000 ) ) ;
#13615 = CARTESIAN_POINT ( 'NONE',  ( 4.996003610813208850E-14, -120.0000000000001137, -25.00000000000000000 ) ) ;
#13616 = FACE_OUTER_BOUND ( 'NONE', #17236, .T. ) ;
#13617 = CARTESIAN_POINT ( 'NONE',  ( 157.9999999999997442, 254.1102501050980322, -45.00000000000000000 ) ) ;
#13619 = EDGE_CURVE ( 'NONE', #26072, #14776, #8796, .T. ) ;
#13618 = CIRCLE ( 'NONE', #15438, 60.59270260175150469 ) ;
#13620 = ORIENTED_EDGE ( 'NONE', *, *, #21874, .F. ) ;
#13621 = CARTESIAN_POINT ( 'NONE',  ( 367.4999999999996021, 44.41075299063184900, 1.850330238640837654E-14 ) ) ;
#13622 = EDGE_CURVE ( 'NONE', #23606, #19624, #469, .T. ) ;
#13623 = B_SPLINE_CURVE_WITH_KNOTS ( 'NONE', 3,
 ( #7871, #20380, #707, #19069, #3835, #10310, #4116, #21221, #5992, #1544, #19208, #12624, #27953, #3688, #14769, #8152, #1682, #27814 ),
 .UNSPECIFIED., .F., .F.,
 ( 4, 2, 2, 2, 2, 2, 2, 2, 4 ),
 ( 0.000000000000000000, 0.006295559550953947446, 0.009443339326430920735, 0.01101722921416940434, 0.01259111910190788969, 0.01888667865286182412, 0.02046056854060030253, 0.02203445842833878440, 0.02518223820381573427 ),
 .UNSPECIFIED. ) ;
#13624 = DIRECTION ( 'NONE',  ( 0.4528218681373709642, -0.8916010070298157064, 0.000000000000000000 ) ) ;
#13625 = DIRECTION ( 'NONE',  ( 3.469446951953614189E-16, -1.000000000000000000, 0.000000000000000000 ) ) ;
#13626 = EDGE_CURVE ( 'NONE', #23386, #2647, #6924, .T. ) ;
#13627 = DIRECTION ( 'NONE',  ( 0.9960550913260672878, 0.000000000000000000, -0.08873699929240111417 ) ) ;
#13628 = AXIS2_PLACEMENT_3D ( 'NONE', #8687, #17441, #11277 ) ;
#13629 = ORIENTED_EDGE ( 'NONE', *, *, #18162, .T. ) ;
#13630 = CARTESIAN_POINT ( 'NONE',  ( 157.4999999999998295, 218.7460624962465090, -45.00000000000000000 ) ) ;
#13631 = EDGE_LOOP ( 'NONE', ( #23915, #15469, #768, #13331 ) ) ;
#13632 = CARTESIAN_POINT ( 'NONE',  ( 158.0000000000007390, 133.7322497447605656, -45.00000000000000000 ) ) ;
#13633 = EDGE_LOOP ( 'NONE', ( #2161, #8428, #28317, #25520 ) ) ;
#13634 = ORIENTED_EDGE ( 'NONE', *, *, #1618, .T. ) ;
#13635 = EDGE_CURVE ( 'NONE', #13747, #22333, #26748, .T. ) ;
#13636 = ORIENTED_EDGE ( 'NONE', *, *, #13454, .F. ) ;
#13637 = ORIENTED_EDGE ( 'NONE', *, *, #10204, .T. ) ;
#13638 = LINE ( 'NONE', #9882, #17306 ) ;
#13639 = CIRCLE ( 'NONE', #26908, 562.1290781602207289 ) ;
#13640 = CARTESIAN_POINT ( 'NONE',  ( -141.6428522700808230, 17.24192588826928585, 83.00000000000001421 ) ) ;
#13641 = DIRECTION ( 'NONE',  ( -0.3102637045530823867, -0.9506505318133460225, 0.000000000000000000 ) ) ;
#13642 = FACE_OUTER_BOUND ( 'NONE', #2573, .T. ) ;
#13643 = DIRECTION ( 'NONE',  ( 0.000000000000000000, -1.000000000000000000, 0.000000000000000000 ) ) ;
#13644 = CARTESIAN_POINT ( 'NONE',  ( -206.8153965817337223, 60.16463287088505751, 19.99797379519356610 ) ) ;
#13645 = CARTESIAN_POINT ( 'NONE',  ( 157.9999999999997442, 249.0945000900840398, 45.00000000000000000 ) ) ;
#13646 = DIRECTION ( 'NONE',  ( 0.000000000000000000, 0.000000000000000000, -1.000000000000000000 ) ) ;
#13647 = FACE_OUTER_BOUND ( 'NONE', #7260, .T. ) ;
#13648 = CARTESIAN_POINT ( 'NONE',  ( -205.8153486680121489, 91.09410686308810057, -26.99305210841084701 ) ) ;
#13649 = DIRECTION ( 'NONE',  ( 0.8916010070293783896, -0.4528218681382319422, 0.000000000000000000 ) ) ;
#13650 = FACE_OUTER_BOUND ( 'NONE', #13368, .T. ) ;
#13651 = LINE ( 'NONE', #569, #18497 ) ;
#13652 = EDGE_CURVE ( 'NONE', #15187, #17412, #22154, .T. ) ;
#13653 = ADVANCED_FACE ( 'NONE', ( #7071 ), #696, .F. ) ;
#13654 = DIRECTION ( 'NONE',  ( -0.000000000000000000, -1.000000000000000000, -0.000000000000000000 ) ) ;
#13655 = FACE_OUTER_BOUND ( 'NONE', #23011, .T. ) ;
#13656 = CARTESIAN_POINT ( 'NONE',  ( 158.0000000000008527, 125.7007497147323818, -45.00000000000000000 ) ) ;
#13657 = LINE ( 'NONE', #3134, #19383 ) ;
#13659 = EDGE_LOOP ( 'NONE', ( #15003, #15101, #28300, #12915 ) ) ;
#13658 = ORIENTED_EDGE ( 'NONE', *, *, #8445, .F. ) ;
#13660 = CARTESIAN_POINT ( 'NONE',  ( -222.0755484219518507, 86.46466326799983904, -17.72675295328876643 ) ) ;
#13661 = VECTOR ( 'NONE', #122, 1000.000000000000000 ) ;
#13662 = LINE ( 'NONE', #7186, #26709 ) ;
#13663 = ORIENTED_EDGE ( 'NONE', *, *, #2013, .F. ) ;
#13664 = CONTEXT_DEPENDENT_SHAPE_REPRESENTATION ( #7077, #11213 ) ;
#13665 = ORIENTED_EDGE ( 'NONE', *, *, #6714, .T. ) ;
#13666 = ORIENTED_EDGE ( 'NONE', *, *, #422, .T. ) ;
#13667 = DIRECTION ( 'NONE',  ( -3.469446951953614189E-16, 1.000000000000000000, 0.000000000000000000 ) ) ;
#13668 = DIRECTION ( 'NONE',  ( -1.000000000000000000, 0.000000000000000000, 0.000000000000000000 ) ) ;
#13669 = EDGE_CURVE ( 'NONE', #3329, #15219, #617, .T. ) ;
#13670 = ORIENTED_EDGE ( 'NONE', *, *, #19382, .T. ) ;
#13671 = VERTEX_POINT ( 'NONE', #7219 ) ;
#13672 = DIRECTION ( 'NONE',  ( 0.000000000000000000, 0.000000000000000000, -1.000000000000000000 ) ) ;
#13673 = VECTOR ( 'NONE', #9925, 1000.000000000000227 ) ;
#13674 = EDGE_CURVE ( 'NONE', #23094, #13728, #15994, .T. ) ;
#13675 = FACE_OUTER_BOUND ( 'NONE', #22835, .T. ) ;
#13676 = ORIENTED_EDGE ( 'NONE', *, *, #8794, .T. ) ;
#13677 = LINE ( 'NONE', #9166, #3157 ) ;
#13678 = AXIS2_PLACEMENT_3D ( 'NONE', #15368, #11044, #23550 ) ;
#13679 = DIRECTION ( 'NONE',  ( 0.000000000000000000, 0.000000000000000000, -1.000000000000000000 ) ) ;
#13680 = VECTOR ( 'NONE', #24086, 1000.000000000000000 ) ;
#13681 = DIRECTION ( 'NONE',  ( -0.000000000000000000, -0.000000000000000000, -1.000000000000000000 ) ) ;
#13682 = EDGE_CURVE ( 'NONE', #20039, #20004, #26597, .T. ) ;
#13683 = CARTESIAN_POINT ( 'NONE',  ( 157.9999999999999432, 211.4763749774776045, 45.00000000000000000 ) ) ;
#13684 = CARTESIAN_POINT ( 'NONE',  ( -208.1368626653883780, 75.14204529818155720, -39.73078884062161364 ) ) ;
#13685 = EDGE_CURVE ( 'NONE', #2005, #12217, #5048, .T. ) ;
#13686 = ORIENTED_EDGE ( 'NONE', *, *, #9908, .F. ) ;
#13687 = DIRECTION ( 'NONE',  ( -0.8916010070295820045, 0.4528218681378310406, 0.000000000000000000 ) ) ;
#13688 = EDGE_CURVE ( 'NONE', #2661, #8764, #182, .T. ) ;
#13689 = CARTESIAN_POINT ( 'NONE',  ( -216.6285193170544972, 139.2238166778980712, -12.99999999956374452 ) ) ;
#13690 = DIRECTION ( 'NONE',  ( 1.000000000000000000, 0.000000000000000000, -0.000000000000000000 ) ) ;
#13691 = CARTESIAN_POINT ( 'NONE',  ( 158.0000000000000853, 196.4291249324366504, -45.00000000000000000 ) ) ;
#13692 = ORIENTED_EDGE ( 'NONE', *, *, #24931, .T. ) ;
#13693 = DIRECTION ( 'NONE',  ( 0.000000000000000000, 0.000000000000000000, -1.000000000000000000 ) ) ;
#13694 = CONICAL_SURFACE ( 'NONE', #24219, 16.36034929305424512, 0.08885387018394150238 ) ;
#13695 = DIRECTION ( 'NONE',  ( -0.000000000000000000, 1.000000000000000000, -1.387778780781445429E-16 ) ) ;
#13696 = AXIS2_PLACEMENT_3D ( 'NONE', #12832, #25885, #1889 ) ;
#13697 = CARTESIAN_POINT ( 'NONE',  ( -142.1532754773451757, 70.11332714433679314, 82.89218380363524830 ) ) ;
#13698 = ORIENTED_EDGE ( 'NONE', *, *, #18052, .T. ) ;
#13699 = ORIENTED_EDGE ( 'NONE', *, *, #1822, .F. ) ;
#13700 = CARTESIAN_POINT ( 'NONE',  ( 87.74278500247204704, 111.0010834413667453, 71.13281249985656984 ) ) ;
#13701 = CARTESIAN_POINT ( 'NONE',  ( 157.9999999999996305, 283.6968751876750616, -45.00000000000000000 ) ) ;
#13702 = ORIENTED_EDGE ( 'NONE', *, *, #5201, .T. ) ;
#13703 = ORIENTED_EDGE ( 'NONE', *, *, #20192, .F. ) ;
#13704 = FACE_OUTER_BOUND ( 'NONE', #22351, .T. ) ;
#13705 = FACE_OUTER_BOUND ( 'NONE', #28322, .T. ) ;
#13706 = AXIS2_PLACEMENT_3D ( 'NONE', #7002, #14192, #20784 ) ;
#13707 = VERTEX_POINT ( 'NONE', #753 ) ;
#13708 = DIRECTION ( 'NONE',  ( -0.8916010070299571488, 0.4528218681370923537, 0.000000000000000000 ) ) ;
#13709 = ORIENTED_EDGE ( 'NONE', *, *, #25622, .F. ) ;
#13710 = FACE_BOUND ( 'NONE', #25640, .T. ) ;
#13711 = AXIS2_PLACEMENT_3D ( 'NONE', #533, #9296, #18061 ) ;
#13712 = EDGE_CURVE ( 'NONE', #15645, #4667, #9661, .T. ) ;
#13713 = VECTOR ( 'NONE', #58, 1000.000000000000000 ) ;
#13714 = LINE ( 'NONE', #22884, #1166 ) ;
#13715 = CARTESIAN_POINT ( 'NONE',  ( -270.1025481742786951, -91.18033988749901653, 0.000000000000000000 ) ) ;
#13716 = CARTESIAN_POINT ( 'NONE',  ( -23.68577686495459389, 129.3251568248628587, -16.93270094945798832 ) ) ;
#13717 = CARTESIAN_POINT ( 'NONE',  ( 154.8288972274760908, 222.6105238444010297, -45.00000000000000000 ) ) ;
#13718 = DIRECTION ( 'NONE',  ( -0.000000000000000000, 1.000000000000000000, -1.387778780781445429E-16 ) ) ;
#13719 = LINE ( 'NONE', #9543, #17094 ) ;
#13720 = EDGE_LOOP ( 'NONE', ( #7072, #21816, #20041, #15929 ) ) ;
#13721 = CARTESIAN_POINT ( 'NONE',  ( 111.9999999999999574, 220.9999999999996874, 45.00000000000000000 ) ) ;
#13722 = ADVANCED_FACE ( 'NONE', ( #16408 ), #27575, .F. ) ;
#13723 = CARTESIAN_POINT ( 'NONE',  ( -295.0000000000002274, -152.0000000000000284, -59.99999999999986500 ) ) ;
#13724 = PLANE ( 'NONE',  #15096 ) ;
#13725 = DIRECTION ( 'NONE',  ( -0.000000000000000000, -0.000000000000000000, -1.000000000000000000 ) ) ;
#13726 = VERTEX_POINT ( 'NONE', #18690 ) ;
#13727 = LINE ( 'NONE', #14016, #9141 ) ;
#13728 = VERTEX_POINT ( 'NONE', #20703 ) ;
#13729 = EDGE_CURVE ( 'NONE', #27008, #19224, #17228, .T. ) ;
#13730 = VECTOR ( 'NONE', #17025, 1000.000000000000000 ) ;
#13731 = DIRECTION ( 'NONE',  ( -0.8916010070294200229, -0.4528218681381501742, 0.000000000000000000 ) ) ;
#13732 = CARTESIAN_POINT ( 'NONE',  ( -210.0000000000000284, 59.99999999999993605, -17.29233506344264626 ) ) ;
#13733 = CARTESIAN_POINT ( 'NONE',  ( 140.6935016229380722, 249.4551793339562096, -143.0663072493378536 ) ) ;
#13734 = ORIENTED_EDGE ( 'NONE', *, *, #10876, .T. ) ;
#13735 = PRESENTATION_STYLE_ASSIGNMENT (( #16448 ) ) ;
#13736 = ORIENTED_EDGE ( 'NONE', *, *, #585, .F. ) ;
#13737 = AXIS2_PLACEMENT_3D ( 'NONE', #19106, #10070, #7907 ) ;
#13738 = DIRECTION ( 'NONE',  ( 0.000000000000000000, 0.000000000000000000, 1.000000000000000000 ) ) ;
#13739 = ORIENTED_EDGE ( 'NONE', *, *, #8766, .F. ) ;
#13740 = CARTESIAN_POINT ( 'NONE',  ( 93.75313621282120380, 240.3341199031587507, 8.151442483331582167 ) ) ;
#13741 = AXIS2_PLACEMENT_3D ( 'NONE', #23876, #12974, #4751 ) ;
#13742 = EDGE_LOOP ( 'NONE', ( #11002, #5515 ) ) ;
#13743 = ORIENTED_EDGE ( 'NONE', *, *, #23750, .F. ) ;
#13744 = FACE_OUTER_BOUND ( 'NONE', #3987, .T. ) ;
#13745 = ORIENTED_EDGE ( 'NONE', *, *, #3111, .T. ) ;
#13746 = ORIENTED_EDGE ( 'NONE', *, *, #570, .T. ) ;
#13747 = VERTEX_POINT ( 'NONE', #3452 ) ;
#13748 = CARTESIAN_POINT ( 'NONE',  ( 107.1040180392210743, 249.6169203092825626, 26.84244457533995742 ) ) ;
#13749 = EDGE_CURVE ( 'NONE', #17968, #10903, #17683, .T. ) ;
#13750 = AXIS2_PLACEMENT_3D ( 'NONE', #8232, #3491, #21437 ) ;
#13751 = CARTESIAN_POINT ( 'NONE',  ( -222.0211651016020085, 135.7213904098416322, 12.97555235349485514 ) ) ;
#13752 = VECTOR ( 'NONE', #27946, 1000.000000000000114 ) ;
#13753 = DIRECTION ( 'NONE',  ( 0.8916010070291696676, 0.4528218681386429467, 0.000000000000000000 ) ) ;
#13754 = DIRECTION ( 'NONE',  ( -0.000000000000000000, -0.000000000000000000, -1.000000000000000000 ) ) ;
#13755 = CIRCLE ( 'NONE', #4533, 6.000000000000005329 ) ;
#13756 = DIRECTION ( 'NONE',  ( 0.7440215159219103480, 0.6681556583950049033, -0.000000000000000000 ) ) ;
#13757 = DIRECTION ( 'NONE',  ( 0.000000000000000000, 0.000000000000000000, -1.000000000000000000 ) ) ;
#13758 = CARTESIAN_POINT ( 'NONE',  ( 157.9999999999998010, 236.5551250525490161, 45.00000000000000000 ) ) ;
#13759 = DIRECTION ( 'NONE',  ( 0.000000000000000000, 0.000000000000000000, 1.000000000000000000 ) ) ;
#13760 = DIRECTION ( 'NONE',  ( 1.000000000000000000, 0.000000000000000000, 0.000000000000000000 ) ) ;
#13761 = DIRECTION ( 'NONE',  ( -0.000000000000000000, -0.000000000000000000, -1.000000000000000000 ) ) ;
#13762 = CARTESIAN_POINT ( 'NONE',  ( 157.4999999999998579, 115.9231871884577174, 45.00000000000000000 ) ) ;
#13763 = ORIENTED_EDGE ( 'NONE', *, *, #22716, .T. ) ;
#13764 = CARTESIAN_POINT ( 'NONE',  ( 155.4185842870420799, 209.3660254037844481, 45.00000000000000000 ) ) ;
#13765 = VECTOR ( 'NONE', #1989, 1000.000000000000114 ) ;
#13766 = EDGE_CURVE ( 'NONE', #12684, #14756, #3170, .T. ) ;
#13767 = ADVANCED_FACE ( 'NONE', ( #2902 ), #14393, .F. ) ;
#13768 = DIRECTION ( 'NONE',  ( -0.000000000000000000, 0.000000000000000000, -1.000000000000000000 ) ) ;
#13769 = DIRECTION ( 'NONE',  ( -0.3102637045530683979, 0.9506505318133506854, 0.000000000000000000 ) ) ;
#13770 = DIRECTION ( 'NONE',  ( 0.000000000000000000, 0.000000000000000000, 1.000000000000000000 ) ) ;
#13771 = VERTEX_POINT ( 'NONE', #7363 ) ;
#13772 = AXIS2_PLACEMENT_3D ( 'NONE', #10350, #5614, #7775 ) ;
#13773 = CARTESIAN_POINT ( 'NONE',  ( 158.0000000000003411, 175.8582498648732440, 45.00000000000000000 ) ) ;
#13774 = ORIENTED_EDGE ( 'NONE', *, *, #14015, .T. ) ;
#13775 = CARTESIAN_POINT ( 'NONE',  ( -310.0000000000001137, -157.0000000000000284, -59.99999999999987210 ) ) ;
#13776 = EDGE_CURVE ( 'NONE', #4340, #24009, #7778, .T. ) ;
#13777 = ORIENTED_EDGE ( 'NONE', *, *, #16658, .T. ) ;
#13778 = AXIS2_PLACEMENT_3D ( 'NONE', #26960, #22517, #26823 ) ;
#13779 = EDGE_CURVE ( 'NONE', #9244, #11167, #5336, .T. ) ;
#13780 = ORIENTED_EDGE ( 'NONE', *, *, #18540, .T. ) ;
#13781 = ORIENTED_EDGE ( 'NONE', *, *, #20410, .F. ) ;
#13782 = ORIENTED_EDGE ( 'NONE', *, *, #19827, .F. ) ;
#13783 = CARTESIAN_POINT ( 'NONE',  ( -189.8086322075389774, 92.49158130768422836, -15.00000000000000000 ) ) ;
#13784 = VECTOR ( 'NONE', #2925, 1000.000000000000000 ) ;
#13785 = DIRECTION ( 'NONE',  ( 0.000000000000000000, 0.000000000000000000, 1.000000000000000000 ) ) ;
#13786 = CARTESIAN_POINT ( 'NONE',  ( -5.421010862427522170E-17, 0.000000000000000000, 0.000000000000000000 ) ) ;
#13787 = CARTESIAN_POINT ( 'NONE',  ( -100.2451658495067477, 134.3005718521120286, -15.54624248649205853 ) ) ;
#13788 = EDGE_CURVE ( 'NONE', #10864, #8063, #7643, .T. ) ;
#13789 = UNCERTAINTY_MEASURE_WITH_UNIT (LENGTH_MEASURE( 1.000000000000000082E-05 ), #15284, 'distance_accuracy_value', 'NONE');
#13790 = CARTESIAN_POINT ( 'NONE',  ( 157.4999999999995453, 206.2066874587088989, -45.00000000000000000 ) ) ;
#13791 = CARTESIAN_POINT ( 'NONE',  ( -214.2384622483376688, 55.08766841006207926, 45.11431866370089239 ) ) ;
#13792 = PLANE ( 'NONE',  #14165 ) ;
#13793 = DIRECTION ( 'NONE',  ( -0.8916010070293383105, -0.4528218681383106015, 0.000000000000000000 ) ) ;
#13794 = CIRCLE ( 'NONE', #10104, 17.93072811908088937 ) ;
#13795 = DIRECTION ( 'NONE',  ( 0.000000000000000000, 0.000000000000000000, -1.000000000000000000 ) ) ;
#13796 = CARTESIAN_POINT ( 'NONE',  ( -228.6461399146356257, 91.02766744526201137, -13.29913430599589219 ) ) ;
#13797 = DIRECTION ( 'NONE',  ( 0.000000000000000000, 8.881784197001253901E-15, 1.000000000000000000 ) ) ;
#13798 = DIRECTION ( 'NONE',  ( 0.000000000000000000, 0.000000000000000000, -1.000000000000000000 ) ) ;
#13799 = FACE_OUTER_BOUND ( 'NONE', #27082, .T. ) ;
#13800 = CIRCLE ( 'NONE', #26601, 32.49120955644046660 ) ;
#13801 = CARTESIAN_POINT ( 'NONE',  ( -6.675997603934725078, 131.5976059255800408, 16.20004726215371704 ) ) ;
#13802 = LINE ( 'NONE', #9620, #25199 ) ;
#13803 = LINE ( 'NONE', #17661, #22082 ) ;
#13804 = DIRECTION ( 'NONE',  ( 1.000000000000000000, 0.000000000000000000, 0.000000000000000000 ) ) ;
#13806 = VERTEX_POINT ( 'NONE', #22588 ) ;
#13805 = ORIENTED_EDGE ( 'NONE', *, *, #4995, .T. ) ;
#13807 = DIRECTION ( 'NONE',  ( 0.8916010070299171808, 0.4528218681371710685, 0.000000000000000000 ) ) ;
#13808 = FACE_OUTER_BOUND ( 'NONE', #1839, .T. ) ;
#13809 = VERTEX_POINT ( 'NONE', #9520 ) ;
#13810 = ORIENTED_EDGE ( 'NONE', *, *, #18339, .F. ) ;
#13811 = VERTEX_POINT ( 'NONE', #5473 ) ;
#13812 = FACE_OUTER_BOUND ( 'NONE', #21784, .T. ) ;
#13813 = VECTOR ( 'NONE', #913, 1000.000000000000114 ) ;
#13814 = CARTESIAN_POINT ( 'NONE',  ( -148.8594576708775037, 124.1404238845194357, 19.51865504791162564 ) ) ;
#13815 = ORIENTED_EDGE ( 'NONE', *, *, #13892, .T. ) ;
#13816 = ORIENTED_EDGE ( 'NONE', *, *, #14231, .F. ) ;
#13817 = CARTESIAN_POINT ( 'NONE',  ( -167.5793538779647918, 116.3743944715606204, -25.89383771362038544 ) ) ;
#13818 = FACE_OUTER_BOUND ( 'NONE', #14110, .T. ) ;
#13819 = ADVANCED_FACE ( 'NONE', ( #1306 ), #11687, .T. ) ;
#13820 = AXIS2_PLACEMENT_3D ( 'NONE', #30, #28171, #26310 ) ;
#13821 = CARTESIAN_POINT ( 'NONE',  ( 158.0000000000005400, 155.7952498048169048, -45.00000000000000000 ) ) ;
#13822 = ORIENTED_EDGE ( 'NONE', *, *, #17613, .T. ) ;
#13823 = EDGE_CURVE ( 'NONE', #14497, #27805, #20563, .T. ) ;
#13824 = CARTESIAN_POINT ( 'NONE',  ( -204.4116019472746473, 91.57545976731941550, 29.21054719826555868 ) ) ;
#13825 = CARTESIAN_POINT ( 'NONE',  ( 87.50000000000029843, 230.0000000000000284, -15.95262490344447492 ) ) ;
#13826 = FACE_OUTER_BOUND ( 'NONE', #28281, .T. ) ;
#13827 = DIRECTION ( 'NONE',  ( -0.000000000000000000, -1.000000000000000000, -0.000000000000000000 ) ) ;
#13828 = CARTESIAN_POINT ( 'NONE',  ( -213.1074610084601773, 72.43174512725769887, -29.09741138161720642 ) ) ;
#13829 = CIRCLE ( 'NONE', #6013, 7.499999999999992895 ) ;
#13830 = DIRECTION ( 'NONE',  ( 0.000000000000000000, 0.000000000000000000, -1.000000000000000000 ) ) ;
#13831 = DIRECTION ( 'NONE',  ( -0.8916010070294909662, -0.4528218681380102306, 0.000000000000000000 ) ) ;
#13832 = DIRECTION ( 'NONE',  ( 1.000000000000000000, 0.000000000000000000, 0.000000000000000000 ) ) ;
#13833 = DIRECTION ( 'NONE',  ( -0.6681556583950049033, 0.7440215159219103480, 0.000000000000000000 ) ) ;
#13834 = ORIENTED_EDGE ( 'NONE', *, *, #6764, .F. ) ;
#13835 = FACE_OUTER_BOUND ( 'NONE', #6047, .T. ) ;
#13836 = VECTOR ( 'NONE', #11952, 1000.000000000000000 ) ;
#13837 = ADVANCED_FACE ( 'NONE', ( #23148 ), #3311, .F. ) ;
#13838 = CARTESIAN_POINT ( 'NONE',  ( -244.5479615644635487, 75.99513337129094737, 15.00000000000000000 ) ) ;
#13839 = DIRECTION ( 'NONE',  ( 0.000000000000000000, -1.000000000000000000, 0.000000000000000000 ) ) ;
#13840 = VERTEX_POINT ( 'NONE', #20424 ) ;
#13841 = ORIENTED_EDGE ( 'NONE', *, *, #8120, .T. ) ;
#13842 = CARTESIAN_POINT ( 'NONE',  ( 157.4999999999996874, 271.4114376538935289, 45.00000000000000000 ) ) ;
#13843 = DIRECTION ( 'NONE',  ( -0.8916010070293383105, -0.4528218681383106015, 0.000000000000000000 ) ) ;
#13844 = EDGE_LOOP ( 'NONE', ( #4916, #10227, #832, #21593, #6043, #16381, #11657, #24528 ) ) ;
#13845 = EDGE_CURVE ( 'NONE', #12991, #26678, #20981, .T. ) ;
#13846 = ORIENTED_EDGE ( 'NONE', *, *, #12618, .F. ) ;
#13847 = EDGE_CURVE ( 'NONE', #20397, #14251, #18416, .T. ) ;
#13848 = FACE_OUTER_BOUND ( 'NONE', #4123, .T. ) ;
#13849 = EDGE_CURVE ( 'NONE', #12468, #4808, #22283, .T. ) ;
#13850 = CIRCLE ( 'NONE', #12002, 20.24534822868278994 ) ;
#13851 = DIRECTION ( 'NONE',  ( 0.000000000000000000, -1.000000000000000000, 0.000000000000000000 ) ) ;
#13852 = EDGE_CURVE ( 'NONE', #7620, #17770, #10075, .T. ) ;
#13853 = CARTESIAN_POINT ( 'NONE',  ( 134.9999999999998579, 220.0000000000000284, -99.00000000000001421 ) ) ;
#13854 = ORIENTED_EDGE ( 'NONE', *, *, #278, .F. ) ;
#13855 = DIRECTION ( 'NONE',  ( 0.000000000000000000, 0.000000000000000000, -1.000000000000000000 ) ) ;
#13856 = ORIENTED_EDGE ( 'NONE', *, *, #5887, .T. ) ;
#13857 = VECTOR ( 'NONE', #9559, 1000.000000000000114 ) ;
#13858 = DIRECTION ( 'NONE',  ( 0.000000000000000000, 0.000000000000000000, -1.000000000000000000 ) ) ;
#13859 = AXIS2_PLACEMENT_3D ( 'NONE', #4129, #12634, #10321 ) ;
#13860 = CARTESIAN_POINT ( 'NONE',  ( -338.3377857851766635, -170.0000000000000853, -110.0000000000000284 ) ) ;
#13861 = CARTESIAN_POINT ( 'NONE',  ( -70.31278697424053803, 101.4626071723526195, -152.5098566583459672 ) ) ;
#13862 = CARTESIAN_POINT ( 'NONE',  ( -1.123482218186120596, 135.6325438607385649, -15.26633278495360635 ) ) ;
#13863 = CARTESIAN_POINT ( 'NONE',  ( 158.0000000000016769, 47.95662448201407102, -45.00000000000000000 ) ) ;
#13864 = CARTESIAN_POINT ( 'NONE',  ( -261.2610864772255468, -166.7207794580371853, -89.99999999999990052 ) ) ;
#13865 = DIRECTION ( 'NONE',  ( 0.000000000000000000, 0.000000000000000000, -1.000000000000000000 ) ) ;
#13866 = ORIENTED_EDGE ( 'NONE', *, *, #11403, .F. ) ;
#13867 = PLANE ( 'NONE',  #12769 ) ;
#13868 = CARTESIAN_POINT ( 'NONE',  ( -229.2498027451139251, 132.0565166830976693, 15.00000000000000000 ) ) ;
#13869 = FACE_OUTER_BOUND ( 'NONE', #3989, .T. ) ;
#13870 = LINE ( 'NONE', #9827, #5697 ) ;
#13871 = ORIENTED_EDGE ( 'NONE', *, *, #18128, .F. ) ;
#13872 = CARTESIAN_POINT ( 'NONE',  ( -235.5935699371920293, 67.74125567661748448, 5.863186529791164503 ) ) ;
#13873 = ORIENTED_EDGE ( 'NONE', *, *, #1145, .T. ) ;
#13874 = VECTOR ( 'NONE', #6386, 1000.000000000000000 ) ;
#13875 = CARTESIAN_POINT ( 'NONE',  ( 112.4999999999998863, 220.0000000000000284, 84.99999999999995737 ) ) ;
#13876 = LINE ( 'NONE', #17880, #4131 ) ;
#13877 = CARTESIAN_POINT ( 'NONE',  ( 137.1196823444857671, 249.9255760664107413, -150.6165463336313053 ) ) ;
#13878 = VERTEX_POINT ( 'NONE', #12667 ) ;
#13879 = DIRECTION ( 'NONE',  ( -0.000000000000000000, 0.000000000000000000, 1.000000000000000000 ) ) ;
#13880 = VECTOR ( 'NONE', #23192, 1000.000000000000227 ) ;
#13881 = ORIENTED_EDGE ( 'NONE', *, *, #25090, .F. ) ;
#13882 = EDGE_CURVE ( 'NONE', #18977, #12684, #2069, .T. ) ;
#13883 = TOROIDAL_SURFACE ( 'NONE', #6981, -538.1631314933625845, 562.1290781602207289 ) ;
#13884 = EDGE_CURVE ( 'NONE', #15785, #4808, #19981, .T. ) ;
#13885 = DIRECTION ( 'NONE',  ( -0.8916010070298157064, -0.4528218681373708532, 0.000000000000000000 ) ) ;
#13886 = EDGE_LOOP ( 'NONE', ( #9633, #27968, #8973, #18046 ) ) ;
#13887 = FACE_OUTER_BOUND ( 'NONE', #24649, .T. ) ;
#13888 = EDGE_LOOP ( 'NONE', ( #10607, #27444 ) ) ;
#13889 = ORIENTED_EDGE ( 'NONE', *, *, #20063, .F. ) ;
#13890 = CARTESIAN_POINT ( 'NONE',  ( 232.4749999999995964, 133.0668745871126930, 36.86484227207694886 ) ) ;
#13891 = ORIENTED_EDGE ( 'NONE', *, *, #1721, .F. ) ;
#13892 = EDGE_CURVE ( 'NONE', #24666, #14722, #21409, .T. ) ;
#13893 = ORIENTED_EDGE ( 'NONE', *, *, #27103, .T. ) ;
#13894 = ORIENTED_EDGE ( 'NONE', *, *, #21810, .F. ) ;
#13895 = TOROIDAL_SURFACE ( 'NONE', #15323, 79.71075545852265520, 9.999999999999996447 ) ;
#13896 = CARTESIAN_POINT ( 'NONE',  ( 109.2338094452269246, 254.3984564255594591, 35.27666983503019082 ) ) ;
#13897 = EDGE_CURVE ( 'NONE', #2501, #19721, #16331, .T. ) ;
#13898 = AXIS2_PLACEMENT_3D ( 'NONE', #16264, #16403, #9373 ) ;
#13899 = CARTESIAN_POINT ( 'NONE',  ( -28.05246235954390244, 188.0718642840173516, 12.99999999999999822 ) ) ;
#13900 = DIRECTION ( 'NONE',  ( 0.8660254037844432595, 0.4999999999999919509, -0.000000000000000000 ) ) ;
#13901 = VECTOR ( 'NONE', #17815, 1000.000000000000000 ) ;
#13902 = VECTOR ( 'NONE', #1900, 1000.000000000000000 ) ;
#13903 = LINE ( 'NONE', #25216, #23422 ) ;
#13904 = CARTESIAN_POINT ( 'NONE',  ( 158.0000000000006537, 141.2558747672816821, 45.00000000000000000 ) ) ;
#13905 = PLANE ( 'NONE',  #6097 ) ;
#13906 = DIRECTION ( 'NONE',  ( 0.8660254037844432595, 0.4999999999999919509, -0.000000000000000000 ) ) ;
#13907 = DIRECTION ( 'NONE',  ( 1.000000000000000000, 0.000000000000000000, -0.000000000000000000 ) ) ;
#13908 = CARTESIAN_POINT ( 'NONE',  ( -262.6917462842096143, -171.5696242569879075, 109.9616379985420167 ) ) ;
#13909 = DIRECTION ( 'NONE',  ( 0.8660254037844432595, 0.4999999999999919509, -0.000000000000000000 ) ) ;
#13910 = DIRECTION ( 'NONE',  ( -0.8916010070300285362, -0.4528218681369517995, 0.000000000000000000 ) ) ;
#13911 = VERTEX_POINT ( 'NONE', #23285 ) ;
#13912 = DIRECTION ( 'NONE',  ( 1.000000000000000000, 0.000000000000000000, 0.000000000000000000 ) ) ;
#13913 = CARTESIAN_POINT ( 'NONE',  ( 217.4999999999996305, 44.41075299063183479, 100.0000000000000142 ) ) ;
#13914 = DIRECTION ( 'NONE',  ( 0.000000000000000000, 0.000000000000000000, -1.000000000000000000 ) ) ;
#13915 = ORIENTED_EDGE ( 'NONE', *, *, #912, .F. ) ;
#13916 = AXIS2_PLACEMENT_3D ( 'NONE', #20936, #3258, #9884 ) ;
#13917 = EDGE_CURVE ( 'NONE', #15896, #19755, #8484, .T. ) ;
#13918 = AXIS2_PLACEMENT_3D ( 'NONE', #26558, #23852, #6887 ) ;
#13919 = CARTESIAN_POINT ( 'NONE',  ( 115.1711027725237528, 222.6105238444006886, 45.00000000000000000 ) ) ;
#13920 = ORIENTED_EDGE ( 'NONE', *, *, #6850, .T. ) ;
#13921 = CARTESIAN_POINT ( 'NONE',  ( 158.0000000000013642, 78.05112457209858690, 45.00000000000000000 ) ) ;
#13922 = AXIS2_PLACEMENT_3D ( 'NONE', #6735, #10773, #25847 ) ;
#13923 = ORIENTED_EDGE ( 'NONE', *, *, #14468, .T. ) ;
#13924 = VECTOR ( 'NONE', #26386, 1000.000000000000000 ) ;
#13925 = ORIENTED_EDGE ( 'NONE', *, *, #4980, .F. ) ;
#13926 = ORIENTED_EDGE ( 'NONE', *, *, #4655, .F. ) ;
#13927 = ORIENTED_EDGE ( 'NONE', *, *, #9816, .T. ) ;
#13928 = CARTESIAN_POINT ( 'NONE',  ( -135.2376737518963807, 129.6700313254847856, 15.43675878823252035 ) ) ;
#13929 = DIRECTION ( 'NONE',  ( 0.8916010070294498879, -0.4528218681380914434, 0.000000000000000000 ) ) ;
#13930 = CARTESIAN_POINT ( 'NONE',  ( 67.86343429515802939, -22.14858123305036486, 45.00000000000000000 ) ) ;
#13931 = B_SPLINE_CURVE_WITH_KNOTS ( 'NONE', 3,
 ( #18715, #7941, #27745, #27463, #12130, #5922, #23594, #14694, #8082, #16847, #3762, #12551, #6062, #23030, #1192, #20873, #7803, #25323, #5645, #14095, #731, #24861, #13817, #20543, #14372, #18670 ),
 .UNSPECIFIED., .F., .F.,
 ( 4, 2, 2, 2, 2, 2, 2, 2, 2, 2, 2, 2, 4 ),
 ( 0.000000000000000000, 0.003366647192498294170, 0.006733294384996588340, 0.01346658876999323913, 0.01683323596249157797, 0.02019988315498991160, 0.02188320675123906975, 0.02356653034748822442, 0.02693317753998661010, 0.03366647192498332941, 0.04039976630998005913, 0.04713306069497678885, 0.05386635507997350469 ),
 .UNSPECIFIED. ) ;
#13932 = EDGE_CURVE ( 'NONE', #8030, #4661, #1723, .T. ) ;
#13933 = ADVANCED_FACE ( 'NONE', ( #8055 ), #19255, .F. ) ;
#13934 = CARTESIAN_POINT ( 'NONE',  ( 157.4999999999998579, 166.0806873385985796, 45.00000000000000000 ) ) ;
#13935 = DIRECTION ( 'NONE',  ( 0.3897722486529259234, -0.9209112846414913012, -1.118268497331688440E-16 ) ) ;
#13936 = AXIS2_PLACEMENT_3D ( 'NONE', #1739, #10659, #14977 ) ;
#13937 = CARTESIAN_POINT ( 'NONE',  ( -194.2411556039511709, 63.21395545898181467, 45.39084185613187827 ) ) ;
#13938 = DIRECTION ( 'NONE',  ( -0.000000000000000000, -0.000000000000000000, -1.000000000000000000 ) ) ;
#13939 = CARTESIAN_POINT ( 'NONE',  ( 367.4999999999996021, 44.41075299063183479, 100.0000000000000284 ) ) ;
#13940 = VECTOR ( 'NONE', #14566, 1000.000000000000000 ) ;
#13941 = CARTESIAN_POINT ( 'NONE',  ( 5.999999999999998224, 0.000000000000000000, -8.000000000000000000 ) ) ;
#13942 = CARTESIAN_POINT ( 'NONE',  ( 157.9999999999997726, 244.0787500750700474, 45.00000000000000000 ) ) ;
#13943 = VECTOR ( 'NONE', #12345, 1000.000000000000000 ) ;
#13944 = DIRECTION ( 'NONE',  ( -0.000000000000000000, -0.000000000000000000, -1.000000000000000000 ) ) ;
#13945 = DIRECTION ( 'NONE',  ( -0.8916010070293515222, 0.4528218681382848443, 0.000000000000000000 ) ) ;
#13946 = DIRECTION ( 'NONE',  ( 1.000000000000000000, 0.000000000000000000, 0.000000000000000000 ) ) ;
#13947 = EDGE_CURVE ( 'NONE', #11388, #969, #21697, .T. ) ;
#13948 = ADVANCED_FACE ( 'NONE', ( #27718 ), #7347, .T. ) ;
#13949 = CARTESIAN_POINT ( 'NONE',  ( -210.0000000000000284, 59.99999999999993605, -17.29233506344264626 ) ) ;
#13950 = FACE_OUTER_BOUND ( 'NONE', #19548, .T. ) ;
#13951 = LINE ( 'NONE', #11928, #16648 ) ;
#13953 = EDGE_LOOP ( 'NONE', ( #19681, #6164, #19230, #18419 ) ) ;
#13952 = EDGE_LOOP ( 'NONE', ( #26820, #5912, #4476, #4341 ) ) ;
#13954 = LINE ( 'NONE', #13512, #19242 ) ;
#13955 = DIRECTION ( 'NONE',  ( -0.9985600561963485777, -0.05364526231779759985, 0.000000000000000000 ) ) ;
#13956 = ORIENTED_EDGE ( 'NONE', *, *, #21988, .T. ) ;
#13957 = VECTOR ( 'NONE', #2737, 1000.000000000000000 ) ;
#13958 = ORIENTED_EDGE ( 'NONE', *, *, #5735, .F. ) ;
#13959 = AXIS2_PLACEMENT_3D ( 'NONE', #7218, #18136, #15992 ) ;
#13960 = LINE ( 'NONE', #9497, #9742 ) ;
#13961 = CARTESIAN_POINT ( 'NONE',  ( 372.9108539694884144, -5.589247009368160768, 100.0000000000000426 ) ) ;
#13962 = ORIENTED_EDGE ( 'NONE', *, *, #11215, .F. ) ;
#13963 = VECTOR ( 'NONE', #9549, 1000.000000000000000 ) ;
#13964 = ORIENTED_EDGE ( 'NONE', *, *, #9908, .T. ) ;
#13965 = CARTESIAN_POINT ( 'NONE',  ( 157.4999999999998579, 65.76568703831686946, 45.00000000000000000 ) ) ;
#13966 = DIRECTION ( 'NONE',  ( 1.530283246943720875E-16, -1.000000000000000000, 0.000000000000000000 ) ) ;
#13967 = EDGE_CURVE ( 'NONE', #16893, #1362, #3919, .T. ) ;
#13968 = ADVANCED_FACE ( 'NONE', ( #1586 ), #10354, .F. ) ;
#13969 = DIRECTION ( 'NONE',  ( 0.9784193629480785193, -0.2066290158914672881, 0.000000000000000000 ) ) ;
#13970 = DIRECTION ( 'NONE',  ( -0.8916010070296530587, 0.4528218681376912080, 0.000000000000000000 ) ) ;
#13971 = LINE ( 'NONE', #22718, #28183 ) ;
#13972 = CARTESIAN_POINT ( 'NONE',  ( 157.4999999999998579, 118.4310621959647563, -45.00000000000000000 ) ) ;
#13973 = CARTESIAN_POINT ( 'NONE',  ( -215.0107612850210899, 71.82996193033663701, -26.64107447012230878 ) ) ;
#13974 = AXIS2_PLACEMENT_3D ( 'NONE', #23980, #24126, #13076 ) ;
#13975 = EDGE_CURVE ( 'NONE', #4392, #17424, #3879, .T. ) ;
#13976 = CARTESIAN_POINT ( 'NONE',  ( 158.0000000000003695, 171.3503748573662051, 45.00000000000000000 ) ) ;
#13977 = DIRECTION ( 'NONE',  ( 0.000000000000000000, 0.000000000000000000, -1.000000000000000000 ) ) ;
#13978 = CARTESIAN_POINT ( 'NONE',  ( 157.9999999999998579, 221.0000000000000284, 45.00000000000000000 ) ) ;
#13979 = AXIS2_PLACEMENT_3D ( 'NONE', #23737, #12835, #1892 ) ;
#13980 = CARTESIAN_POINT ( 'NONE',  ( 157.4999999999997442, 253.8563126013445697, 45.00000000000000000 ) ) ;
#13981 = ORIENTED_EDGE ( 'NONE', *, *, #16393, .F. ) ;
#13982 = EDGE_CURVE ( 'NONE', #11176, #14709, #20106, .T. ) ;
#13983 = CARTESIAN_POINT ( 'NONE',  ( 142.6536686473015152, 238.4775906502254941, -45.00000000000000000 ) ) ;
#13984 = EDGE_CURVE ( 'NONE', #18505, #5660, #6468, .T. ) ;
#13985 = CARTESIAN_POINT ( 'NONE',  ( -244.5479615644635487, 75.99513337129094737, 5.000000000000002665 ) ) ;
#13986 = CARTESIAN_POINT ( 'NONE',  ( -160.0000000000000284, 59.99999999999994316, 15.00000000000000000 ) ) ;
#13987 = ORIENTED_EDGE ( 'NONE', *, *, #10519, .T. ) ;
#13988 = ADVANCED_FACE ( 'NONE', ( #2431 ), #19685, .F. ) ;
#13989 = EDGE_LOOP ( 'NONE', ( #14821, #9776, #13834, #2654 ) ) ;
#13990 = CARTESIAN_POINT ( 'NONE',  ( 96.92716526683047107, 115.1868982021512124, 77.49999999971905140 ) ) ;
#13991 = CARTESIAN_POINT ( 'NONE',  ( 158.0000000000015632, 55.98812451204224061, 45.00000000000000000 ) ) ;
#13992 = EDGE_LOOP ( 'NONE', ( #16519, #1417, #3681, #25162 ) ) ;
#13993 = CIRCLE ( 'NONE', #12614, 10.53396790234565117 ) ;
#13994 = VERTEX_POINT ( 'NONE', #4446 ) ;
#13995 = DIRECTION ( 'NONE',  ( -0.000000000000000000, -0.000000000000000000, -1.000000000000000000 ) ) ;
#13996 = CARTESIAN_POINT ( 'NONE',  ( -205.1370039499190625, 144.1304017549904586, -15.00000000000000000 ) ) ;
#13997 = EDGE_LOOP ( 'NONE', ( #27276, #22644, #25298, #23301, #26606, #1701, #18946, #13337 ) ) ;
#13998 = FACE_OUTER_BOUND ( 'NONE', #27373, .T. ) ;
#13999 = ORIENTED_EDGE ( 'NONE', *, *, #26497, .T. ) ;
#14000 = AXIS2_PLACEMENT_3D ( 'NONE', #25788, #27930, #28073 ) ;
#14001 = LINE ( 'NONE', #25172, #1968 ) ;
#14002 = CARTESIAN_POINT ( 'NONE',  ( 157.4999999999998579, 221.2539375037535194, 45.00000000000000000 ) ) ;
#14003 = DIRECTION ( 'NONE',  ( -1.000000000000000000, -0.000000000000000000, 0.000000000000000000 ) ) ;
#14004 = CARTESIAN_POINT ( 'NONE',  ( -27.07984315909205009, 129.1630299464794405, -16.99514979029525108 ) ) ;
#14005 = DIRECTION ( 'NONE',  ( 0.8916010070293510781, -0.4528218681382856770, 0.000000000000000000 ) ) ;
#14006 = LINE ( 'NONE', #11418, #485 ) ;
#14007 = LINE ( 'NONE', #3198, #5637 ) ;
#14008 = ORIENTED_EDGE ( 'NONE', *, *, #27343, .F. ) ;
#14009 = PLANE ( 'NONE',  #14144 ) ;
#14010 = VECTOR ( 'NONE', #23481, 1000.000000000000000 ) ;
#14011 = LINE ( 'NONE', #9826, #8799 ) ;
#14012 = FACE_BOUND ( 'NONE', #18758, .T. ) ;
#14013 = EDGE_LOOP ( 'NONE', ( #4840, #28004, #16144, #18969 ) ) ;
#14014 = VECTOR ( 'NONE', #15660, 1000.000000000000000 ) ;
#14015 = EDGE_CURVE ( 'NONE', #27002, #25971, #3001, .T. ) ;
#14016 = CARTESIAN_POINT ( 'NONE',  ( 197.6424708188942816, 64.50455043276784295, -45.00000000000000000 ) ) ;
#14017 = EDGE_CURVE ( 'NONE', #15637, #10398, #10924, .T. ) ;
#14018 = VERTEX_POINT ( 'NONE', #7 ) ;
#14019 = EDGE_CURVE ( 'NONE', #24937, #17953, #4587, .T. ) ;
#14020 = CARTESIAN_POINT ( 'NONE',  ( 89.99999999999988631, 240.0000000000000284, -45.00000000000000000 ) ) ;
#14021 = DIRECTION ( 'NONE',  ( 0.8916010070293783896, -0.4528218681382319422, 0.000000000000000000 ) ) ;
#14022 = DIRECTION ( 'NONE',  ( 0.000000000000000000, 0.000000000000000000, 1.000000000000000000 ) ) ;
#14023 = ORIENTED_EDGE ( 'NONE', *, *, #18403, .T. ) ;
#14024 = CARTESIAN_POINT ( 'NONE',  ( -21.33210486176665910, 0.000000000000000000, 100.0000000000000000 ) ) ;
#14025 = LINE ( 'NONE', #5375, #10682 ) ;
#14026 = CIRCLE ( 'NONE', #10781, 10.00000000000000888 ) ;
#14027 = ORIENTED_EDGE ( 'NONE', *, *, #18015, .F. ) ;
#14028 = CARTESIAN_POINT ( 'NONE',  ( 134.9999999999998579, 220.0000000000000284, -119.9999999999999858 ) ) ;
#14029 = CARTESIAN_POINT ( 'NONE',  ( 97.40125796617704168, 241.4156732773147667, 11.01277537798790007 ) ) ;
#14030 = ORIENTED_EDGE ( 'NONE', *, *, #2322, .T. ) ;
#14031 = VERTEX_POINT ( 'NONE', #6746 ) ;
#14032 = DIRECTION ( 'NONE',  ( -0.8916010070293383105, -0.4528218681383106015, 0.000000000000000000 ) ) ;
#14033 = ORIENTED_EDGE ( 'NONE', *, *, #7094, .F. ) ;
#14034 = AXIS2_PLACEMENT_3D ( 'NONE', #10095, #15228, #5494 ) ;
#14035 = VERTEX_POINT ( 'NONE', #7040 ) ;
#14036 = ORIENTED_EDGE ( 'NONE', *, *, #7974, .F. ) ;
#14037 = VECTOR ( 'NONE', #5260, 1000.000000000000000 ) ;
#14038 = FACE_OUTER_BOUND ( 'NONE', #392, .T. ) ;
#14039 = DIRECTION ( 'NONE',  ( 1.000000000000000000, 0.000000000000000000, 0.000000000000000000 ) ) ;
#14040 = DIRECTION ( 'NONE',  ( -0.000000000000000000, -0.000000000000000000, 1.000000000000000000 ) ) ;
#14041 = CIRCLE ( 'NONE', #2543, 5.999999999999991118 ) ;
#14042 = DIRECTION ( 'NONE',  ( 1.000000000000000000, 0.000000000000000000, 0.000000000000000000 ) ) ;
#14043 = DIRECTION ( 'NONE',  ( 0.000000000000000000, 0.000000000000000000, 1.000000000000000000 ) ) ;
#14044 = LINE ( 'NONE', #18615, #21212 ) ;
#14045 = LINE ( 'NONE', #9580, #11324 ) ;
#14046 = DIRECTION ( 'NONE',  ( 1.000000000000000000, 1.530283246943720628E-16, 0.000000000000000000 ) ) ;
#14047 = CARTESIAN_POINT ( 'NONE',  ( -268.1131488955604141, -165.6689427093874372, 109.3643454197753897 ) ) ;
#14048 = CARTESIAN_POINT ( 'NONE',  ( 150.5563491861038870, 236.9705627484768797, 45.00000000000000000 ) ) ;
#14049 = CARTESIAN_POINT ( 'NONE',  ( 115.1343022193454004, 209.3890158820094314, -98.75454612047968794 ) ) ;
#14050 = ORIENTED_EDGE ( 'NONE', *, *, #422, .F. ) ;
#14051 = EDGE_CURVE ( 'NONE', #7786, #7612, #8044, .T. ) ;
#14052 = ADVANCED_FACE ( 'NONE', ( #26420 ), #1289, .T. ) ;
#14053 = CARTESIAN_POINT ( 'NONE',  ( 0.6601832576049850854, -1.250000000000000444, 7.428391153593997487 ) ) ;
#14054 = LINE ( 'NONE', #1238, #3405 ) ;
#14055 = CIRCLE ( 'NONE', #1635, 1.999999999999993339 ) ;
#14056 = CARTESIAN_POINT ( 'NONE',  ( -146.6428522700808230, 74.54464929955099706, 80.00000000000001421 ) ) ;
#14057 = ORIENTED_EDGE ( 'NONE', *, *, #18084, .T. ) ;
#14058 = AXIS2_PLACEMENT_3D ( 'NONE', #6667, #10984, #20018 ) ;
#14059 = CARTESIAN_POINT ( 'NONE',  ( 157.4999999999998579, 78.30506207585207790, -45.00000000000000000 ) ) ;
#14060 = ORIENTED_EDGE ( 'NONE', *, *, #14287, .T. ) ;
#14061 = AXIS2_PLACEMENT_3D ( 'NONE', #2136, #26272, #15376 ) ;
#14062 = VERTEX_POINT ( 'NONE', #26091 ) ;
#14063 = VERTEX_POINT ( 'NONE', #6421 ) ;
#14064 = ORIENTED_EDGE ( 'NONE', *, *, #6850, .F. ) ;
#14065 = ORIENTED_EDGE ( 'NONE', *, *, #28147, .T. ) ;
#14066 = CARTESIAN_POINT ( 'NONE',  ( -67.47855672616037737, 135.5178657931547832, 13.65870838648359964 ) ) ;
#14067 = DIRECTION ( 'NONE',  ( 0.8916010070297852863, 0.4528218681374306942, 0.000000000000000000 ) ) ;
#14068 = DIRECTION ( 'NONE',  ( 1.000000000000000000, 1.850371707708594316E-16, -0.000000000000000000 ) ) ;
#14069 = CARTESIAN_POINT ( 'NONE',  ( -90.16297593177748126, 134.7821557438530533, -15.45724512967298026 ) ) ;
#14070 = CIRCLE ( 'NONE', #25071, 4.355764593064429313 ) ;
#14071 = CARTESIAN_POINT ( 'NONE',  ( 134.9999999999998579, 171.5103103742661688, 84.99999999999995737 ) ) ;
#14072 = CARTESIAN_POINT ( 'NONE',  ( -194.7277720219268815, 63.01928361507884091, 39.96465835449415493 ) ) ;
#14073 = FACE_OUTER_BOUND ( 'NONE', #14930, .T. ) ;
#14074 = EDGE_CURVE ( 'NONE', #5015, #14898, #23953, .T. ) ;
#14075 = CARTESIAN_POINT ( 'NONE',  ( 157.9999999999997158, 256.6181251126050711, 45.00000000000000000 ) ) ;
#14076 = CARTESIAN_POINT ( 'NONE',  ( 79.99999999999997158, 81.96349540849362825, -100.0000000000000284 ) ) ;
#14077 = CARTESIAN_POINT ( 'NONE',  ( -221.0514588393455142, 88.12431193532715668, -15.86718054107228859 ) ) ;
#14078 = VECTOR ( 'NONE', #4825, 1000.000000000000000 ) ;
#14079 = CARTESIAN_POINT ( 'NONE',  ( -254.3350114625770289, -91.18033988749901653, 0.000000000000000000 ) ) ;
#14080 = DIRECTION ( 'NONE',  ( 0.000000000000000000, 0.000000000000000000, 1.000000000000000000 ) ) ;
#14081 = ADVANCED_FACE ( 'NONE', ( #13420 ), #12862, .F. ) ;
#14082 = CARTESIAN_POINT ( 'NONE',  ( -76.25760768171835480, 219.6666220619077876, -15.00000000000000000 ) ) ;
#14083 = CARTESIAN_POINT ( 'NONE',  ( 111.0641325991587252, 99.15168937823352735, -100.0000000000000142 ) ) ;
#14084 = DIRECTION ( 'NONE',  ( 1.000000000000000000, 0.000000000000000000, 0.000000000000000000 ) ) ;
#14086 = VERTEX_POINT ( 'NONE', #24324 ) ;
#14085 = ORIENTED_EDGE ( 'NONE', *, *, #8743, .T. ) ;
#14087 = EDGE_CURVE ( 'NONE', #26198, #19256, #23657, .T. ) ;
#14088 = LINE ( 'NONE', #25126, #25342 ) ;
#14089 = VERTEX_POINT ( 'NONE', #26055 ) ;
#14090 = VECTOR ( 'NONE', #12573, 1000.000000000000000 ) ;
#14091 = ORIENTED_EDGE ( 'NONE', *, *, #25333, .F. ) ;
#14092 = DIRECTION ( 'NONE',  ( -1.000000000000000000, 0.000000000000000000, 0.000000000000000000 ) ) ;
#14093 = ORIENTED_EDGE ( 'NONE', *, *, #3507, .T. ) ;
#14094 = ORIENTED_EDGE ( 'NONE', *, *, #12095, .T. ) ;
#14095 = CARTESIAN_POINT ( 'NONE',  ( -174.9473576776401842, 112.5984928542032151, -28.94822812299444337 ) ) ;
#14096 = EDGE_CURVE ( 'NONE', #14325, #28186, #8682, .T. ) ;
#14097 = PLANE ( 'NONE',  #20072 ) ;
#14098 = DIRECTION ( 'NONE',  ( 0.000000000000000000, 0.000000000000000000, -1.000000000000000000 ) ) ;
#14099 = DIRECTION ( 'NONE',  ( 0.8916010070293710621, -0.4528218681382463195, 0.000000000000000000 ) ) ;
#14100 = ADVANCED_FACE ( 'NONE', ( #22176 ), #6798, .F. ) ;
#14101 = DIRECTION ( 'NONE',  ( -0.8916010070293584056, 0.4528218681382713551, 0.000000000000000000 ) ) ;
#14102 = DIRECTION ( 'NONE',  ( 0.8916010070297542001, -0.4528218681374919230, 0.000000000000000000 ) ) ;
#14103 = VECTOR ( 'NONE', #19123, 1000.000000000000227 ) ;
#14104 = CARTESIAN_POINT ( 'NONE',  ( -202.1528982378773946, 60.83080389531252763, -24.93098023360007431 ) ) ;
#14105 = CLOSED_SHELL ( 'NONE', ( #24733, #24368, #15472, #5519, #11628, #16035, #25271, #9322, #21577, #19402, #23662, #2507, #2166, #3759, #7594, #6782, #28238, #19055, #8248, #26199, #18302, #20481, #1083, #13037, #8532, #4475, #14113, #19363, #20226, #16117, #19569, #3512, #18600, #24825, #1844, #4686, #315, #5742, #3376, #2232, #1341, #343, #23568, #5838, #27586, #27731, #12367, #26459, #6452, #2075, #6617, #14823, #24245, #4669, #11849, #22203, #2732, #23695, #24865, #10603, #9650, #20395, #11294, #11903, #11707, #13767, #20183, #12441, #13837, #11245, #19049, #22356, #14230, #25555, #21271, #8585 ) ) ;
#14106 = LINE ( 'NONE', #18407, #20123 ) ;
#14107 = DIRECTION ( 'NONE',  ( -1.000000000000000000, -8.673617379884036705E-17, 0.000000000000000000 ) ) ;
#14108 = CARTESIAN_POINT ( 'NONE',  ( -138.6428522700808230, 71.54464929955099706, 83.00000000000001421 ) ) ;
#14109 = DIRECTION ( 'NONE',  ( 0.000000000000000000, -1.000000000000000000, 0.000000000000000000 ) ) ;
#14110 = EDGE_LOOP ( 'NONE', ( #9165, #18594, #1392, #19185 ) ) ;
#14111 = DIRECTION ( 'NONE',  ( -1.000000000000000000, -0.000000000000000000, -0.000000000000000000 ) ) ;
#14112 = EDGE_CURVE ( 'NONE', #13260, #5560, #6378, .T. ) ;
#14113 = ADVANCED_FACE ( 'NONE', ( #17576 ), #19313, .F. ) ;
#14114 = CARTESIAN_POINT ( 'NONE',  ( -231.1655399901254384, 65.02775169233193253, 6.844214734954432444 ) ) ;
#14115 = CARTESIAN_POINT ( 'NONE',  ( -156.8436863811591593, 180.7779002010535692, 12.99999999999999822 ) ) ;
#14116 = VERTEX_POINT ( 'NONE', #8815 ) ;
#14117 = DIRECTION ( 'NONE',  ( -1.000000000000000000, 0.000000000000000000, 0.000000000000000000 ) ) ;
#14118 = VERTEX_POINT ( 'NONE', #28056 ) ;
#14119 = CARTESIAN_POINT ( 'NONE',  ( 109.9999999999999147, 140.0000000000000000, 90.00000000000002842 ) ) ;
#14120 = CARTESIAN_POINT ( 'NONE',  ( 158.0000000000009663, 113.1613746771971876, -45.00000000000000000 ) ) ;
#14121 = ORIENTED_EDGE ( 'NONE', *, *, #16816, .T. ) ;
#14122 = AXIS2_PLACEMENT_3D ( 'NONE', #11485, #11633, #11337 ) ;
#14124 = ADVANCED_FACE ( 'NONE', ( #2062 ), #6238, .T. ) ;
#14123 = ORIENTED_EDGE ( 'NONE', *, *, #3333, .F. ) ;
#14125 = DIRECTION ( 'NONE',  ( 1.000000000000000000, -0.000000000000000000, -0.000000000000000000 ) ) ;
#14126 = CIRCLE ( 'NONE', #1714, 55.86582179324592090 ) ;
#14127 = CARTESIAN_POINT ( 'NONE',  ( -76.25760768171836901, 154.8982798170083299, -15.00000000000000000 ) ) ;
#14128 = CARTESIAN_POINT ( 'NONE',  ( -273.6211430000234373, -91.18033988749901653, 0.000000000000000000 ) ) ;
#14129 = ORIENTED_EDGE ( 'NONE', *, *, #12256, .T. ) ;
#14130 = LINE ( 'NONE', #4917, #23368 ) ;
#14131 = ORIENTED_EDGE ( 'NONE', *, *, #2663, .F. ) ;
#14132 = CARTESIAN_POINT ( 'NONE',  ( 158.0000000000008242, 128.2086247222394206, 45.00000000000000000 ) ) ;
#14133 = EDGE_CURVE ( 'NONE', #606, #5551, #4219, .T. ) ;
#14134 = PLANE ( 'NONE',  #21346 ) ;
#14135 = EDGE_CURVE ( 'NONE', #5095, #83, #10838, .T. ) ;
#14136 = CARTESIAN_POINT ( 'NONE',  ( 372.9108539694884144, 19.41075299063184900, 95.49671038392668265 ) ) ;
#14137 = CARTESIAN_POINT ( 'NONE',  ( 4.490032364213274008, 138.9202551321229464, -13.09535261425119224 ) ) ;
#14138 = CARTESIAN_POINT ( 'NONE',  ( 157.4999999999994884, 211.2224374737238577, 45.00000000000000000 ) ) ;
#14139 = CARTESIAN_POINT ( 'NONE',  ( 157.4999999999997158, 261.3799376238655441, 45.00000000000000000 ) ) ;
#14140 = DIRECTION ( 'NONE',  ( 0.4528218681372321863, 0.8916010070298862056, -0.000000000000000000 ) ) ;
#14141 = VECTOR ( 'NONE', #6307, 1000.000000000000000 ) ;
#14142 = ORIENTED_EDGE ( 'NONE', *, *, #22893, .F. ) ;
#14143 = PLANE ( 'NONE',  #9084 ) ;
#14144 = AXIS2_PLACEMENT_3D ( 'NONE', #11422, #496, #4788 ) ;
#14145 = SHAPE_REPRESENTATION ( 'slotted cheese head screw_iso_ISO 1207 - M10 x 35 - 35N', ( #10637 ), #25313 ) ;
#14146 = CARTESIAN_POINT ( 'NONE',  ( 157.4999999999998579, 168.5885623461056184, 45.00000000000000000 ) ) ;
#14147 = CARTESIAN_POINT ( 'NONE',  ( -124.9781469243919076, 222.2250949724356985, 5.000000000000002665 ) ) ;
#14148 = ORIENTED_EDGE ( 'NONE', *, *, #4426, .T. ) ;
#14149 = CARTESIAN_POINT ( 'NONE',  ( -242.2383635333241898, 73.34843395317835757, 5.047097023363151358 ) ) ;
#14150 = ORIENTED_EDGE ( 'NONE', *, *, #7076, .T. ) ;
#14151 = DIRECTION ( 'NONE',  ( -0.8379557447115514313, 0.5457381880580733924, 0.000000000000000000 ) ) ;
#14152 = CARTESIAN_POINT ( 'NONE',  ( -66.57029700917655646, 102.2156118568357783, 45.00000000000000000 ) ) ;
#14153 = CARTESIAN_POINT ( 'NONE',  ( 115.1711027725237955, 217.3894761555985156, 45.00000000000000000 ) ) ;
#14154 = VERTEX_POINT ( 'NONE', #13149 ) ;
#14155 = DIRECTION ( 'NONE',  ( 0.8916010070299774659, -0.4528218681370523302, 0.000000000000000000 ) ) ;
#14156 = DIRECTION ( 'NONE',  ( -0.5555587585212683477, -0.8314772792026894344, 0.000000000000000000 ) ) ;
#14157 = ORIENTED_EDGE ( 'NONE', *, *, #27411, .T. ) ;
#14158 = CARTESIAN_POINT ( 'NONE',  ( -81.41884555190407013, 134.7389654164047386, 15.46487976177122015 ) ) ;
#14159 = CARTESIAN_POINT ( 'NONE',  ( 95.84672108982582017, 240.8689139502125158, 9.670646206302331294 ) ) ;
#14160 = ORIENTED_EDGE ( 'NONE', *, *, #12735, .T. ) ;
#14161 = EDGE_LOOP ( 'NONE', ( #19888, #21151, #6787, #24540 ) ) ;
#14162 = LINE ( 'NONE', #2949, #24641 ) ;
#14163 = VERTEX_POINT ( 'NONE', #17157 ) ;
#14164 = CIRCLE ( 'NONE', #15534, 10.71881775658151170 ) ;
#14165 = AXIS2_PLACEMENT_3D ( 'NONE', #22686, #19948, #22539 ) ;
#14166 = ORIENTED_EDGE ( 'NONE', *, *, #27771, .T. ) ;
#14167 = ORIENTED_EDGE ( 'NONE', *, *, #8120, .F. ) ;
#14168 = EDGE_CURVE ( 'NONE', #16763, #23612, #14041, .T. ) ;
#14169 = CARTESIAN_POINT ( 'NONE',  ( 108.2753065237184984, 248.3531133182649739, 34.86527342666781237 ) ) ;
#14170 = EDGE_CURVE ( 'NONE', #28088, #14580, #23765, .T. ) ;
#14171 = CARTESIAN_POINT ( 'NONE',  ( 157.9999999999997158, 258.6181251126050711, 45.00000000000000000 ) ) ;
#14172 = CARTESIAN_POINT ( 'NONE',  ( -218.8273392347298341, 140.3457761587514767, -14.99191580167117266 ) ) ;
#14173 = CARTESIAN_POINT ( 'NONE',  ( 88.58553289623264959, 111.2425746091564491, -71.46484375013500312 ) ) ;
#14174 = CARTESIAN_POINT ( 'NONE',  ( 232.4999999999996305, 133.0668745871126930, 36.86484227207694886 ) ) ;
#14175 = DIRECTION ( 'NONE',  ( 0.5555587585212703461, 0.8314772792026879911, -9.637408206913768347E-16 ) ) ;
#14176 = AXIS2_PLACEMENT_3D ( 'NONE', #3664, #12454, #14461 ) ;
#14177 = LINE ( 'NONE', #20203, #1669 ) ;
#14178 = DIRECTION ( 'NONE',  ( -0.000000000000000000, -0.000000000000000000, -1.000000000000000000 ) ) ;
#14179 = DIRECTION ( 'NONE',  ( 1.000000000000000000, 0.000000000000000000, 0.000000000000000000 ) ) ;
#14180 = DIRECTION ( 'NONE',  ( 1.000000000000000000, -0.000000000000000000, -0.000000000000000000 ) ) ;
#14181 = ORIENTED_EDGE ( 'NONE', *, *, #7673, .T. ) ;
#14182 = AXIS2_PLACEMENT_3D ( 'NONE', #25778, #27922, #28065 ) ;
#14183 = AXIS2_PLACEMENT_3D ( 'NONE', #14657, #5882, #7768 ) ;
#14184 = CARTESIAN_POINT ( 'NONE',  ( 93.75311240682748348, 240.3341156238397218, -8.151427701230094414 ) ) ;
#14185 = CARTESIAN_POINT ( 'NONE',  ( 18.34304381486422741, 88.89403053572398505, 98.65506662663811710 ) ) ;
#14186 = CARTESIAN_POINT ( 'NONE',  ( 157.4999999999998579, 188.6515624061619576, -45.00000000000000000 ) ) ;
#14187 = ORIENTED_EDGE ( 'NONE', *, *, #13514, .F. ) ;
#14188 = AXIS2_PLACEMENT_3D ( 'NONE', #6621, #4598, #9360 ) ;
#14189 = DIRECTION ( 'NONE',  ( 1.000000000000000000, 0.000000000000000000, -0.000000000000000000 ) ) ;
#14190 = EDGE_LOOP ( 'NONE', ( #25129, #14883, #11227, #6296 ) ) ;
#14191 = EDGE_CURVE ( 'NONE', #10929, #21594, #21606, .T. ) ;
#14192 = DIRECTION ( 'NONE',  ( -0.6343833064826058799, 0.7730186417261851739, 0.000000000000000000 ) ) ;
#14193 = ORIENTED_EDGE ( 'NONE', *, *, #22375, .T. ) ;
#14194 = VECTOR ( 'NONE', #19008, 1000.000000000000000 ) ;
#14195 = VERTEX_POINT ( 'NONE', #4491 ) ;
#14196 = AXIS2_PLACEMENT_3D ( 'NONE', #20716, #5209, #5064 ) ;
#14197 = ORIENTED_EDGE ( 'NONE', *, *, #13626, .T. ) ;
#14198 = EDGE_CURVE ( 'NONE', #7226, #11653, #15880, .T. ) ;
#14199 = VERTEX_POINT ( 'NONE', #26194 ) ;
#14200 = FACE_OUTER_BOUND ( 'NONE', #4134, .T. ) ;
#14201 = LINE ( 'NONE', #3541, #15976 ) ;
#14202 = CARTESIAN_POINT ( 'NONE',  ( 157.4999999999998579, 90.84443711338730054, -45.00000000000000000 ) ) ;
#14203 = EDGE_CURVE ( 'NONE', #9208, #4554, #10981, .T. ) ;
#14204 = EDGE_CURVE ( 'NONE', #2585, #20893, #2338, .T. ) ;
#14205 = CIRCLE ( 'NONE', #8218, 4.999999999999995559 ) ;
#14206 = ADVANCED_FACE ( 'NONE', ( #24475 ), #6065, .T. ) ;
#14207 = CARTESIAN_POINT ( 'NONE',  ( -62.70704562728440834, 133.3662835691973214, -15.73207420746911289 ) ) ;
#14208 = CIRCLE ( 'NONE', #18326, 10.71881775658151170 ) ;
#14209 = CARTESIAN_POINT ( 'NONE',  ( 157.9999999999996874, 264.1417501351260171, -45.00000000000000000 ) ) ;
#14210 = CARTESIAN_POINT ( 'NONE',  ( -214.1250002713545086, 55.22895589251825754, 44.08339233875913976 ) ) ;
#14211 = CARTESIAN_POINT ( 'NONE',  ( -210.0000000000000568, -210.8114316696540982, 90.00000000000002842 ) ) ;
#14212 = CARTESIAN_POINT ( 'NONE',  ( -142.3347590520894812, 127.5090500945063070, -16.40665191978878568 ) ) ;
#14213 = CARTESIAN_POINT ( 'NONE',  ( 158.0000000000008242, 128.2086247222394206, 45.00000000000000000 ) ) ;
#14214 = CARTESIAN_POINT ( 'NONE',  ( -203.7172301001751578, 92.58626701197334796, -28.49277624592259528 ) ) ;
#14215 = DIRECTION ( 'NONE',  ( 0.000000000000000000, 0.000000000000000000, 1.000000000000000000 ) ) ;
#14216 = LINE ( 'NONE', #24982, #1529 ) ;
#14217 = ORIENTED_EDGE ( 'NONE', *, *, #5592, .F. ) ;
#14218 = VECTOR ( 'NONE', #20559, 1000.000000000000227 ) ;
#14219 = LINE ( 'NONE', #26854, #26562 ) ;
#14220 = AXIS2_PLACEMENT_3D ( 'NONE', #26830, #24531, #27244 ) ;
#14221 = DIRECTION ( 'NONE',  ( 0.000000000000000000, 0.000000000000000000, 1.000000000000000000 ) ) ;
#14222 = DIRECTION ( 'NONE',  ( 0.000000000000000000, 0.000000000000000000, 1.000000000000000000 ) ) ;
#14224 = ORIENTED_EDGE ( 'NONE', *, *, #14112, .T. ) ;
#14223 = VERTEX_POINT ( 'NONE', #3613 ) ;
#14225 = AXIS2_PLACEMENT_3D ( 'NONE', #10149, #1517, #27649 ) ;
#14226 = PLANE ( 'NONE',  #21669 ) ;
#14227 = VERTEX_POINT ( 'NONE', #17366 ) ;
#14228 = ORIENTED_EDGE ( 'NONE', *, *, #15411, .F. ) ;
#14229 = ORIENTED_EDGE ( 'NONE', *, *, #3549, .F. ) ;
#14230 = ADVANCED_FACE ( 'NONE', ( #16428 ), #22886, .F. ) ;
#14231 = EDGE_CURVE ( 'NONE', #5806, #3147, #18996, .T. ) ;
#14232 = EDGE_CURVE ( 'NONE', #13878, #3041, #10376, .T. ) ;
#14233 = ORIENTED_EDGE ( 'NONE', *, *, #3460, .T. ) ;
#14234 = ORIENTED_EDGE ( 'NONE', *, *, #12329, .T. ) ;
#14235 = DIRECTION ( 'NONE',  ( -0.05364526231778202897, 0.9985600561963492439, 0.000000000000000000 ) ) ;
#14236 = DIRECTION ( 'NONE',  ( 0.000000000000000000, 0.000000000000000000, 1.000000000000000000 ) ) ;
#14237 = VECTOR ( 'NONE', #14040, 1000.000000000000000 ) ;
#14238 = EDGE_CURVE ( 'NONE', #11167, #27470, #10239, .T. ) ;
#14239 = CARTESIAN_POINT ( 'NONE',  ( 109.9999999999999574, -120.0000000000000426, 100.0000000000000142 ) ) ;
#14240 = CARTESIAN_POINT ( 'NONE',  ( 97.56713245600785456, 233.1474958787437970, -20.66394368293470407 ) ) ;
#14241 = VECTOR ( 'NONE', #23461, 1000.000000000000000 ) ;
#14242 = CARTESIAN_POINT ( 'NONE',  ( -210.7172313291012529, 103.7585653882801182, -15.00000000000000000 ) ) ;
#14243 = EDGE_CURVE ( 'NONE', #25694, #16854, #3195, .T. ) ;
#14244 = FACE_OUTER_BOUND ( 'NONE', #19126, .T. ) ;
#14245 = FACE_BOUND ( 'NONE', #24962, .T. ) ;
#14246 = CARTESIAN_POINT ( 'NONE',  ( -217.2638015013723418, 71.38783981852336069, -24.17165906551136700 ) ) ;
#14247 = CARTESIAN_POINT ( 'NONE',  ( 111.0465853079006848, 201.9350282673592858, -149.7646631383025237 ) ) ;
#14248 = DIRECTION ( 'NONE',  ( 4.163336342344337027E-16, -1.000000000000000000, 1.387778780781445429E-16 ) ) ;
#14249 = CARTESIAN_POINT ( 'NONE',  ( 127.3463313526980727, 238.4775906502252667, 45.00000000000000000 ) ) ;
#14250 = PLANE ( 'NONE',  #3388 ) ;
#14251 = VERTEX_POINT ( 'NONE', #1049 ) ;
#14252 = CARTESIAN_POINT ( 'NONE',  ( 118.3245732435423037, 235.1487993679093051, -99.88685888571279747 ) ) ;
#14253 = VECTOR ( 'NONE', #21041, 1000.000000000000000 ) ;
#14254 = DIRECTION ( 'NONE',  ( -0.9985600561963489108, 0.05364526231778980747, 0.000000000000000000 ) ) ;
#14255 = ORIENTED_EDGE ( 'NONE', *, *, #6109, .F. ) ;
#14256 = APPLICATION_PROTOCOL_DEFINITION ( 'draft international standard', 'automotive_design', 1998, #12422 ) ;
#14257 = EDGE_LOOP ( 'NONE', ( #16835, #26327, #22935, #1110 ) ) ;
#14258 = VECTOR ( 'NONE', #8611, 1000.000000000000000 ) ;
#14259 = ADVANCED_FACE ( 'NONE', ( #6453 ), #1188, .F. ) ;
#14260 = CARTESIAN_POINT ( 'NONE',  ( 104.1118574119297762, 122.0584436052485700, 84.84374999969743669 ) ) ;
#14261 = CARTESIAN_POINT ( 'NONE',  ( 157.4999999999997158, 263.8878126313725829, 45.00000000000000000 ) ) ;
#14262 = ORIENTED_EDGE ( 'NONE', *, *, #5594, .T. ) ;
#14263 = ORIENTED_EDGE ( 'NONE', *, *, #26347, .T. ) ;
#14264 = CARTESIAN_POINT ( 'NONE',  ( -160.8326600028555902, 120.2355194873575073, 21.37420696376536711 ) ) ;
#14265 = LINE ( 'NONE', #9530, #632 ) ;
#14266 = DIRECTION ( 'NONE',  ( -0.000000000000000000, 1.000000000000000000, -1.387778780781445429E-16 ) ) ;
#14267 = ORIENTED_EDGE ( 'NONE', *, *, #22948, .T. ) ;
#14268 = CARTESIAN_POINT ( 'NONE',  ( 119.9999999987673220, 136.1131920015923811, 100.0000000000000142 ) ) ;
#14269 = ORIENTED_EDGE ( 'NONE', *, *, #10835, .F. ) ;
#14270 = CARTESIAN_POINT ( 'NONE',  ( -210.0000000000000568, -220.0000000000000853, -109.1217062362807155 ) ) ;
#14271 = EDGE_CURVE ( 'NONE', #16287, #10929, #18852, .T. ) ;
#14272 = VECTOR ( 'NONE', #5295, 1000.000000000000000 ) ;
#14273 = ADVANCED_FACE ( 'NONE', ( #5779 ), #14276, .F. ) ;
#14274 = CARTESIAN_POINT ( 'NONE',  ( 157.4999999999998579, 65.76568703831686946, -45.00000000000000000 ) ) ;
#14275 = DIRECTION ( 'NONE',  ( 0.000000000000000000, -0.000000000000000000, 1.000000000000000000 ) ) ;
#14276 = PLANE ( 'NONE',  #22304 ) ;
#14277 = DIRECTION ( 'NONE',  ( -0.000000000000000000, 1.000000000000000000, -1.387778780781445429E-16 ) ) ;
#14278 = LINE ( 'NONE', #23447, #27117 ) ;
#14279 = VECTOR ( 'NONE', #10071, 1000.000000000000114 ) ;
#14280 = CARTESIAN_POINT ( 'NONE',  ( 163.3898168894218657, 210.3035215302631968, -143.4419542882358201 ) ) ;
#14281 = VERTEX_POINT ( 'NONE', #21001 ) ;
#14282 = FACE_OUTER_BOUND ( 'NONE', #1245, .T. ) ;
#14283 = DIRECTION ( 'NONE',  ( -0.000000000000000000, 0.000000000000000000, -1.000000000000000000 ) ) ;
#14284 = CARTESIAN_POINT ( 'NONE',  ( 232.4999999999996305, 83.06687458711267880, 30.83984227207693607 ) ) ;
#14285 = CARTESIAN_POINT ( 'NONE',  ( -180.0000000000000284, -40.00000000000004974, 25.00000000000000711 ) ) ;
#14286 = ORIENTED_EDGE ( 'NONE', *, *, #6270, .F. ) ;
#14287 = EDGE_CURVE ( 'NONE', #5668, #3350, #21145, .T. ) ;
#14288 = CARTESIAN_POINT ( 'NONE',  ( -234.1469129038714811, 66.78385994367808109, 6.149209796590400678 ) ) ;
#14289 = ORIENTED_EDGE ( 'NONE', *, *, #21100, .T. ) ;
#14290 = ADVANCED_FACE ( 'NONE', ( #18712 ), #1468, .T. ) ;
#14291 = CARTESIAN_POINT ( 'NONE',  ( 157.4999999999997442, 253.8563126013445697, 45.00000000000000000 ) ) ;
#14292 = DIRECTION ( 'NONE',  ( -0.8379557447115656421, -0.5457381880580516320, 0.000000000000000000 ) ) ;
#14293 = ORIENTED_EDGE ( 'NONE', *, *, #19029, .T. ) ;
#14294 = CARTESIAN_POINT ( 'NONE',  ( 158.0000000000005400, 158.3031248123239436, 45.00000000000000000 ) ) ;
#14295 = VERTEX_POINT ( 'NONE', #16565 ) ;
#14296 = AXIS2_PLACEMENT_3D ( 'NONE', #9582, #18755, #11889 ) ;
#14297 = CARTESIAN_POINT ( 'NONE',  ( -134.5347440196730133, 128.5535302534177617, 17.26723801115314316 ) ) ;
#14298 = CARTESIAN_POINT ( 'NONE',  ( 109.8317202412775657, 257.3567735479731482, 40.41962601158171964 ) ) ;
#14299 = ORIENTED_EDGE ( 'NONE', *, *, #19137, .F. ) ;
#14300 = VERTEX_POINT ( 'NONE', #5641 ) ;
#14301 = DIRECTION ( 'NONE',  ( 0.8916010070295922185, -0.4528218681378110566, 0.000000000000000000 ) ) ;
#14302 = ORIENTED_EDGE ( 'NONE', *, *, #6743, .F. ) ;
#14303 = CIRCLE ( 'NONE', #27574, 23.59849023212046149 ) ;
#14304 = ORIENTED_EDGE ( 'NONE', *, *, #9256, .F. ) ;
#14305 = EDGE_LOOP ( 'NONE', ( #4138, #24523, #21272, #2686, #5305 ) ) ;
#14306 = CARTESIAN_POINT ( 'NONE',  ( 157.9999999999998295, 224.0157500150140208, 45.00000000000000000 ) ) ;
#14307 = EDGE_CURVE ( 'NONE', #18107, #25491, #21287, .T. ) ;
#14308 = CARTESIAN_POINT ( 'NONE',  ( 2.399999999999999911, -1.249999999999999112, -7.582700855991164168 ) ) ;
#14309 = CARTESIAN_POINT ( 'NONE',  ( 157.9999999999998579, 219.0000000000000284, 45.00000000000000000 ) ) ;
#14310 = CARTESIAN_POINT ( 'NONE',  ( 105.2480867101029531, 123.6573351780301095, -85.93750000029402258 ) ) ;
#14311 = LINE ( 'NONE', #16194, #19076 ) ;
#14312 = LINE ( 'NONE', #5111, #12990 ) ;
#14313 = VECTOR ( 'NONE', #4789, 1000.000000000000000 ) ;
#14314 = DIRECTION ( 'NONE',  ( -0.000000000000000000, -0.000000000000000000, -1.000000000000000000 ) ) ;
#14315 = CARTESIAN_POINT ( 'NONE',  ( -272.0101343024082325, -170.1474602875829589, 103.5721376568295256 ) ) ;
#14317 = CARTESIAN_POINT ( 'NONE',  ( 33.10302365956999182, 221.6666220619077876, -13.00000000000000000 ) ) ;
#14316 = CIRCLE ( 'NONE', #20718, 5.000000000000004441 ) ;
#14318 = CARTESIAN_POINT ( 'NONE',  ( 158.0000000000001421, 193.4133749174225443, 45.00000000000000000 ) ) ;
#14319 = ORIENTED_EDGE ( 'NONE', *, *, #12611, .T. ) ;
#14320 = CARTESIAN_POINT ( 'NONE',  ( -6.136237936124284253, 131.7900252471816884, 16.14451440323835740 ) ) ;
#14321 = CARTESIAN_POINT ( 'NONE',  ( 109.9999999999998863, 258.9419543489020725, -43.16741111682571130 ) ) ;
#14322 = DIRECTION ( 'NONE',  ( -0.05364526231779676024, -0.9985600561963485777, 0.000000000000000000 ) ) ;
#14323 = DIRECTION ( 'NONE',  ( -0.000000000000000000, -1.000000000000000000, -0.000000000000000000 ) ) ;
#14324 = CARTESIAN_POINT ( 'NONE',  ( 0.000000000000000000, 0.000000000000000000, -45.00000000000000000 ) ) ;
#14325 = VERTEX_POINT ( 'NONE', #12267 ) ;
#14326 = EDGE_CURVE ( 'NONE', #4287, #15447, #1328, .T. ) ;
#14327 = EDGE_CURVE ( 'NONE', #13271, #2501, #6692, .T. ) ;
#14328 = CARTESIAN_POINT ( 'NONE',  ( 157.9999999999998010, 233.5393750375350237, 45.00000000000000000 ) ) ;
#14329 = ORIENTED_EDGE ( 'NONE', *, *, #14639, .F. ) ;
#14330 = DIRECTION ( 'NONE',  ( -0.8916010070299369428, 0.4528218681371322663, 0.000000000000000000 ) ) ;
#14331 = ORIENTED_EDGE ( 'NONE', *, *, #1284, .T. ) ;
#14332 = EDGE_CURVE ( 'NONE', #21244, #27897, #7024, .T. ) ;
#14333 = ORIENTED_EDGE ( 'NONE', *, *, #313, .F. ) ;
#14334 = AXIS2_PLACEMENT_3D ( 'NONE', #4608, #8656, #4757 ) ;
#14335 = ORIENTED_EDGE ( 'NONE', *, *, #11073, .F. ) ;
#14336 = ORIENTED_EDGE ( 'NONE', *, *, #21385, .T. ) ;
#14337 = ORIENTED_EDGE ( 'NONE', *, *, #8884, .T. ) ;
#14338 = CIRCLE ( 'NONE', #2862, 30.00000000000000000 ) ;
#14339 = DIRECTION ( 'NONE',  ( -1.000000000000000000, 0.000000000000000000, 0.000000000000000000 ) ) ;
#14340 = PRODUCT_DEFINITION_FORMATION_WITH_SPECIFIED_SOURCE ( 'ANY', '', #14871, .NOT_KNOWN. ) ;
#14341 = DIRECTION ( 'NONE',  ( 0.000000000000000000, 1.000000000000000000, -0.000000000000000000 ) ) ;
#14342 = PLANE ( 'NONE',  #28082 ) ;
#14343 = AXIS2_PLACEMENT_3D ( 'NONE', #9053, #26563, #15672 ) ;
#14344 = CARTESIAN_POINT ( 'NONE',  ( -96.55704474936557347, 136.1739396949002980, -15.19855580619790025 ) ) ;
#14345 = LINE ( 'NONE', #11779, #15255 ) ;
#14346 = DIRECTION ( 'NONE',  ( -0.8916010070296940260, -0.4528218681376106058, 0.000000000000000000 ) ) ;
#14347 = DIRECTION ( 'NONE',  ( 0.4528218681378710087, -0.8916010070295616874, 0.000000000000000000 ) ) ;
#14348 = FACE_OUTER_BOUND ( 'NONE', #20789, .T. ) ;
#14349 = CARTESIAN_POINT ( 'NONE',  ( -270.8397870484705550, -170.2891267554672936, -93.46372687881502372 ) ) ;
#14350 = FACE_OUTER_BOUND ( 'NONE', #23095, .T. ) ;
#14351 = FACE_OUTER_BOUND ( 'NONE', #4242, .T. ) ;
#14352 = LINE ( 'NONE', #3131, #7947 ) ;
#14353 = EDGE_LOOP ( 'NONE', ( #1611, #10387 ) ) ;
#14354 = AXIS2_PLACEMENT_3D ( 'NONE', #12399, #28014, #21135 ) ;
#14355 = AXIS2_PLACEMENT_3D ( 'NONE', #3275, #17173, #23640 ) ;
#14356 = DIRECTION ( 'NONE',  ( 0.000000000000000000, -1.000000000000000000, -1.214306433183764966E-16 ) ) ;
#14357 = LINE ( 'NONE', #10041, #21627 ) ;
#14358 = EDGE_CURVE ( 'NONE', #20612, #9432, #283, .T. ) ;
#14359 = CARTESIAN_POINT ( 'NONE',  ( 158.0000000000002274, 185.8897498949014278, 45.00000000000000000 ) ) ;
#14360 = CIRCLE ( 'NONE', #5651, 18.46313063346208239 ) ;
#14362 = ORIENTED_EDGE ( 'NONE', *, *, #25574, .T. ) ;
#14361 = ORIENTED_EDGE ( 'NONE', *, *, #3832, .F. ) ;
#14363 = VECTOR ( 'NONE', #21589, 1000.000000000000000 ) ;
#14364 = ADVANCED_FACE ( 'NONE', ( #15808 ), #6879, .F. ) ;
#14365 = FACE_OUTER_BOUND ( 'NONE', #17605, .T. ) ;
#14366 = EDGE_CURVE ( 'NONE', #11107, #23094, #15659, .T. ) ;
#14367 = ORIENTED_EDGE ( 'NONE', *, *, #23498, .T. ) ;
#14368 = ORIENTED_EDGE ( 'NONE', *, *, #6864, .T. ) ;
#14369 = VERTEX_POINT ( 'NONE', #21830 ) ;
#14370 = ORIENTED_EDGE ( 'NONE', *, *, #26305, .F. ) ;
#14371 = EDGE_LOOP ( 'NONE', ( #10763, #21884, #6108, #4775 ) ) ;
#14372 = CARTESIAN_POINT ( 'NONE',  ( -161.9247682478280979, 118.9584040179142761, -23.58860542993421916 ) ) ;
#14373 = AXIS2_PLACEMENT_3D ( 'NONE', #20300, #5066, #24760 ) ;
#14374 = CARTESIAN_POINT ( 'NONE',  ( 158.0000000000006537, 143.2558747672816821, -45.00000000000000000 ) ) ;
#14375 = VECTOR ( 'NONE', #16306, 999.9999999999998863 ) ;
#14376 = CARTESIAN_POINT ( 'NONE',  ( 135.9999999999998295, 242.9999999999997158, -45.00000000000000000 ) ) ;
#14377 = CIRCLE ( 'NONE', #27660, 1.999999999999996891 ) ;
#14378 = AXIS2_PLACEMENT_3D ( 'NONE', #12038, #12181, #7581 ) ;
#14379 = DIRECTION ( 'NONE',  ( -1.000000000000000000, 0.000000000000000000, 0.000000000000000000 ) ) ;
#14380 = CARTESIAN_POINT ( 'NONE',  ( 157.4999999999998579, 98.36806213590843129, -45.00000000000000000 ) ) ;
#14381 = CARTESIAN_POINT ( 'NONE',  ( -210.0000000000000568, -157.0000000000000284, -89.99999999999987210 ) ) ;
#14382 = CARTESIAN_POINT ( 'NONE',  ( 134.9999999999998579, 220.0000000000000284, 100.0000000000000142 ) ) ;
#14383 = ADVANCED_FACE ( 'NONE', ( #13647 ), #11198, .F. ) ;
#14384 = CARTESIAN_POINT ( 'NONE',  ( 109.0192378864665557, 205.0000000000002558, -138.9999999999999432 ) ) ;
#14385 = LINE ( 'NONE', #23143, #10154 ) ;
#14386 = CARTESIAN_POINT ( 'NONE',  ( 158.0000000000014211, 73.03537455708450921, 45.00000000000000000 ) ) ;
#14387 = ORIENTED_EDGE ( 'NONE', *, *, #16341, .F. ) ;
#14388 = AXIS2_PLACEMENT_3D ( 'NONE', #14652, #6167, #23131 ) ;
#14389 = CARTESIAN_POINT ( 'NONE',  ( -203.1779787704217313, 93.05164332230201296, 28.77272332722130699 ) ) ;
#14390 = EDGE_CURVE ( 'NONE', #5230, #22744, #18093, .T. ) ;
#14391 = VECTOR ( 'NONE', #26326, 1000.000000000000114 ) ;
#14392 = EDGE_CURVE ( 'NONE', #3701, #26778, #8897, .T. ) ;
#14393 = PLANE ( 'NONE',  #26857 ) ;
#14394 = ORIENTED_EDGE ( 'NONE', *, *, #1295, .T. ) ;
#14395 = CARTESIAN_POINT ( 'NONE',  ( 238.4999999999996305, 83.06687458711267880, -36.86484227207694175 ) ) ;
#14396 = AXIS2_PLACEMENT_3D ( 'NONE', #22185, #20024, #4932 ) ;
#14397 = VERTEX_POINT ( 'NONE', #2707 ) ;
#14398 = ORIENTED_EDGE ( 'NONE', *, *, #22133, .F. ) ;
#14399 = FACE_OUTER_BOUND ( 'NONE', #189, .T. ) ;
#14400 = CARTESIAN_POINT ( 'NONE',  ( 0.9552291512637774984, 1.249999999999999556, 7.454565938624106991 ) ) ;
#14401 = EDGE_LOOP ( 'NONE', ( #330, #24779, #23834, #23579 ) ) ;
#14402 = ORIENTED_EDGE ( 'NONE', *, *, #26309, .T. ) ;
#14403 = CARTESIAN_POINT ( 'NONE',  ( 88.58553289623264959, 111.2425746091564491, -71.46484375013500312 ) ) ;
#14404 = CARTESIAN_POINT ( 'NONE',  ( 95.56986273107233387, 231.9897703952537995, 19.35213621132750106 ) ) ;
#14405 = CARTESIAN_POINT ( 'NONE',  ( 158.0000000000010516, 105.6377496546760568, 45.00000000000000000 ) ) ;
#14406 = VERTEX_POINT ( 'NONE', #8755 ) ;
#14407 = CARTESIAN_POINT ( 'NONE',  ( 217.4999999999996305, 258.6181251126050711, 6.025000000000016342 ) ) ;
#14408 = EDGE_LOOP ( 'NONE', ( #10582, #4727, #18661, #23121 ) ) ;
#14409 = CONICAL_SURFACE ( 'NONE', #22213, 21.20097097723064294, 0.08885387018394180769 ) ;
#14410 = LINE ( 'NONE', #16146, #17571 ) ;
#14411 = DIRECTION ( 'NONE',  ( -0.000000000000000000, -0.000000000000000000, -1.000000000000000000 ) ) ;
#14412 = DIRECTION ( 'NONE',  ( 0.8790438869537404720, 0.4767408570798813972, -0.000000000000000000 ) ) ;
#14413 = EDGE_CURVE ( 'NONE', #18325, #22419, #19670, .T. ) ;
#14414 = DIRECTION ( 'NONE',  ( -0.000000000000000000, -0.000000000000000000, -1.000000000000000000 ) ) ;
#14415 = TOROIDAL_SURFACE ( 'NONE', #11682, 72.21503689626331379, 5.000000000000000000 ) ;
#14416 = DIRECTION ( 'NONE',  ( 1.000000000000000000, 0.000000000000000000, 0.000000000000000000 ) ) ;
#14417 = FACE_OUTER_BOUND ( 'NONE', #13057, .T. ) ;
#14418 = CARTESIAN_POINT ( 'NONE',  ( 162.7383316901385513, 208.5692331145191076, -149.5158039499305289 ) ) ;
#14419 = EDGE_CURVE ( 'NONE', #14195, #13314, #9041, .T. ) ;
#14420 = VERTEX_POINT ( 'NONE', #11495 ) ;
#14421 = CARTESIAN_POINT ( 'NONE',  ( 134.9999999999998579, -150.0000000000000284, -84.99999999999997158 ) ) ;
#14422 = CARTESIAN_POINT ( 'NONE',  ( 158.0000000000012790, 85.57474959461971764, 45.00000000000000000 ) ) ;
#14423 = CARTESIAN_POINT ( 'NONE',  ( 126.9999999999998579, 404.6636166603179277, -145.0000000000000000 ) ) ;
#14424 = CARTESIAN_POINT ( 'NONE',  ( 158.0000000000013642, 78.05112457209858690, 45.00000000000000000 ) ) ;
#14425 = VERTEX_POINT ( 'NONE', #17654 ) ;
#14426 = CARTESIAN_POINT ( 'NONE',  ( -175.0000000000000000, -120.0000000000001705, 76.02500000000001990 ) ) ;
#14427 = VERTEX_POINT ( 'NONE', #24405 ) ;
#14428 = ADVANCED_FACE ( 'NONE', ( #22108 ), #17793, .T. ) ;
#14429 = CARTESIAN_POINT ( 'NONE',  ( -112.3221550338875687, 22.24192588826928585, 83.00000000000001421 ) ) ;
#14430 = CARTESIAN_POINT ( 'NONE',  ( 20.92655468430566756, 155.3461090732848220, -15.00000000000000000 ) ) ;
#14431 = LINE ( 'NONE', #5797, #19961 ) ;
#14432 = ORIENTED_EDGE ( 'NONE', *, *, #14866, .T. ) ;
#14433 = FACE_OUTER_BOUND ( 'NONE', #11290, .T. ) ;
#14434 = CARTESIAN_POINT ( 'NONE',  ( 157.9999999999998579, 221.5078750075070104, -45.00000000000000000 ) ) ;
#14435 = ORIENTED_EDGE ( 'NONE', *, *, #20600, .F. ) ;
#14436 = AXIS2_PLACEMENT_3D ( 'NONE', #10375, #6059, #23590 ) ;
#14437 = ADVANCED_FACE ( 'NONE', ( #15229 ), #21963, .T. ) ;
#14438 = LINE ( 'NONE', #14574, #13880 ) ;
#14439 = CARTESIAN_POINT ( 'NONE',  ( 109.3255224386495001, 254.7368901578298050, 35.86658157783330836 ) ) ;
#14440 = EDGE_LOOP ( 'NONE', ( #12249, #25836, #24537, #21664 ) ) ;
#14441 = CIRCLE ( 'NONE', #24994, 2.000000000000012879 ) ;
#14442 = ORIENTED_EDGE ( 'NONE', *, *, #11141, .F. ) ;
#14443 = LINE ( 'NONE', #10127, #14090 ) ;
#14444 = ORIENTED_EDGE ( 'NONE', *, *, #11508, .T. ) ;
#14445 = ORIENTED_EDGE ( 'NONE', *, *, #24047, .T. ) ;
#14446 = ORIENTED_EDGE ( 'NONE', *, *, #24142, .T. ) ;
#14447 = EDGE_CURVE ( 'NONE', #4562, #24145, #9330, .T. ) ;
#14448 = CARTESIAN_POINT ( 'NONE',  ( 158.0000000000007674, 133.2243747372535267, 45.00000000000000000 ) ) ;
#14449 = CARTESIAN_POINT ( 'NONE',  ( 157.9999999999998295, 226.5236250225210313, 45.00000000000000000 ) ) ;
#14450 = DIRECTION ( 'NONE',  ( 0.8018642810807399268, 0.5975062131282553590, 0.000000000000000000 ) ) ;
#14451 = VECTOR ( 'NONE', #6170, 1000.000000000000000 ) ;
#14452 = CARTESIAN_POINT ( 'NONE',  ( -43.02437977270766822, 129.7200458115293031, -16.81627168235288394 ) ) ;
#14453 = CARTESIAN_POINT ( 'NONE',  ( 109.9999999999999432, -100.0000000000000142, 25.00000000000000000 ) ) ;
#14454 = EDGE_CURVE ( 'NONE', #16059, #23894, #8995, .T. ) ;
#14455 = LINE ( 'NONE', #1371, #7923 ) ;
#14456 = CARTESIAN_POINT ( 'NONE',  ( 158.0000000000005969, 148.7794997898028271, 45.00000000000000000 ) ) ;
#14457 = FACE_OUTER_BOUND ( 'NONE', #9049, .T. ) ;
#14458 = CARTESIAN_POINT ( 'NONE',  ( 65.00000000000000000, -120.0000000000000995, -63.97499999999998721 ) ) ;
#14459 = CARTESIAN_POINT ( 'NONE',  ( -270.1025481742786951, -91.18033988749901653, 14.95564396479129243 ) ) ;
#14460 = ORIENTED_EDGE ( 'NONE', *, *, #7863, .F. ) ;
#14461 = DIRECTION ( 'NONE',  ( 0.000000000000000000, -1.598721155460225418E-14, 1.000000000000000000 ) ) ;
#14462 = CARTESIAN_POINT ( 'NONE',  ( 101.0657985141824611, 243.3257530605124543, -15.10239625482412507 ) ) ;
#14463 = CARTESIAN_POINT ( 'NONE',  ( 15.23471640472432043, 89.54451151409071485, 98.44134334489216087 ) ) ;
#14464 = FILL_AREA_STYLE_COLOUR ( '', #1296 ) ;
#14465 = CARTESIAN_POINT ( 'NONE',  ( 410.1240808061609187, 61.15703788601284430, -145.0000000000000000 ) ) ;
#14466 = ORIENTED_EDGE ( 'NONE', *, *, #16241, .T. ) ;
#14467 = ADVANCED_FACE ( 'NONE', ( #13218 ), #27330, .T. ) ;
#14468 = EDGE_CURVE ( 'NONE', #8924, #5313, #2275, .T. ) ;
#14469 = CARTESIAN_POINT ( 'NONE',  ( -68.57415822541635464, -18.01420295945611727, 80.00000000000001421 ) ) ;
#14470 = ORIENTED_EDGE ( 'NONE', *, *, #17787, .F. ) ;
#14471 = DIRECTION ( 'NONE',  ( 1.000000000000000000, 0.000000000000000000, 0.000000000000000000 ) ) ;
#14472 = ORIENTED_EDGE ( 'NONE', *, *, #3474, .F. ) ;
#14473 = VECTOR ( 'NONE', #9291, 1000.000000000000000 ) ;
#14474 = VECTOR ( 'NONE', #4826, 1000.000000000000000 ) ;
#14475 = ORIENTED_EDGE ( 'NONE', *, *, #24020, .F. ) ;
#14476 = CARTESIAN_POINT ( 'NONE',  ( -75.08089385218988809, 136.1113822420730912, 13.54512463695272650 ) ) ;
#14477 = VERTEX_POINT ( 'NONE', #19950 ) ;
#14478 = VECTOR ( 'NONE', #5195, 1000.000000000000000 ) ;
#14479 = ORIENTED_EDGE ( 'NONE', *, *, #9420, .T. ) ;
#14480 = DIRECTION ( 'NONE',  ( 0.4528218681382713551, 0.8916010070293584056, -0.000000000000000000 ) ) ;
#14481 = EDGE_CURVE ( 'NONE', #26306, #21594, #4716, .T. ) ;
#14482 = LINE ( 'NONE', #18780, #7700 ) ;
#14483 = LINE ( 'NONE', #5419, #7484 ) ;
#14484 = DIRECTION ( 'NONE',  ( -8.673617379884036705E-17, 1.000000000000000000, 0.000000000000000000 ) ) ;
#14485 = EDGE_CURVE ( 'NONE', #23195, #25296, #25053, .T. ) ;
#14486 = LINE ( 'NONE', #19205, #27963 ) ;
#14487 = LINE ( 'NONE', #11918, #6345 ) ;
#14488 = CARTESIAN_POINT ( 'NONE',  ( -270.0328369100889745, -165.2068861618994902, 88.28012068083718589 ) ) ;
#14489 = DIRECTION ( 'NONE',  ( -0.000000000000000000, -0.000000000000000000, -1.000000000000000000 ) ) ;
#14490 = AXIS2_PLACEMENT_3D ( 'NONE', #8680, #13280, #13147 ) ;
#14491 = DIRECTION ( 'NONE',  ( -0.000000000000000000, 0.000000000000000000, -1.000000000000000000 ) ) ;
#14492 = EDGE_CURVE ( 'NONE', #10929, #15393, #23106, .T. ) ;
#14493 = DIRECTION ( 'NONE',  ( -0.000000000000000000, -0.000000000000000000, 1.000000000000000000 ) ) ;
#14494 = CARTESIAN_POINT ( 'NONE',  ( 217.4749999999996533, 258.6181251126050711, 6.000000000000019540 ) ) ;
#14495 = CARTESIAN_POINT ( 'NONE',  ( 158.0000000000006253, 148.2716247822957882, 45.00000000000000000 ) ) ;
#14496 = AXIS2_PLACEMENT_3D ( 'NONE', #13032, #28355, #17182 ) ;
#14497 = VERTEX_POINT ( 'NONE', #18234 ) ;
#14498 = DIRECTION ( 'NONE',  ( 0.3102637045530823312, 0.9506505318133460225, 0.000000000000000000 ) ) ;
#14499 = CARTESIAN_POINT ( 'NONE',  ( 99.60675733924797726, 85.63108538499818678, -100.0000000000000284 ) ) ;
#14500 = AXIS2_PLACEMENT_3D ( 'NONE', #11346, #26547, #24549 ) ;
#14502 = VERTEX_POINT ( 'NONE', #10032 ) ;
#14501 = VERTEX_POINT ( 'NONE', #981 ) ;
#14503 = DIRECTION ( 'NONE',  ( 0.000000000000000000, 0.000000000000000000, 1.000000000000000000 ) ) ;
#14504 = ORIENTED_EDGE ( 'NONE', *, *, #27376, .F. ) ;
#14505 = ORIENTED_EDGE ( 'NONE', *, *, #8145, .T. ) ;
#14506 = ADVANCED_FACE ( 'NONE', ( #14348 ), #3126, .F. ) ;
#14507 = VERTEX_POINT ( 'NONE', #13941 ) ;
#14508 = VERTEX_POINT ( 'NONE', #12201 ) ;
#14509 = VECTOR ( 'NONE', #10450, 1000.000000000000000 ) ;
#14510 = ORIENTED_EDGE ( 'NONE', *, *, #10766, .T. ) ;
#14511 = ORIENTED_EDGE ( 'NONE', *, *, #23785, .T. ) ;
#14512 = VECTOR ( 'NONE', #3178, 1000.000000000000000 ) ;
#14513 = CARTESIAN_POINT ( 'NONE',  ( -203.2481855153402250, 92.57460631283319685, 29.78692811926998729 ) ) ;
#14514 = FACE_BOUND ( 'NONE', #16474, .T. ) ;
#14515 = VECTOR ( 'NONE', #27230, 1000.000000000000000 ) ;
#14516 = FACE_OUTER_BOUND ( 'NONE', #14161, .T. ) ;
#14517 = EDGE_CURVE ( 'NONE', #18450, #26868, #26983, .T. ) ;
#14518 = EDGE_CURVE ( 'NONE', #18272, #18076, #13133, .T. ) ;
#14519 = CARTESIAN_POINT ( 'NONE',  ( 187.4999999999996305, 0.000000000000000000, 0.000000000000000000 ) ) ;
#14520 = DIRECTION ( 'NONE',  ( -1.000000000000000000, 0.000000000000000000, 0.000000000000000000 ) ) ;
#14521 = FACE_OUTER_BOUND ( 'NONE', #8170, .T. ) ;
#14522 = DIRECTION ( 'NONE',  ( -0.8916010070293783896, -0.4528218681382319422, 0.000000000000000000 ) ) ;
#14523 = DIRECTION ( 'NONE',  ( 0.000000000000000000, 0.000000000000000000, -1.000000000000000000 ) ) ;
#14524 = DIRECTION ( 'NONE',  ( 0.000000000000000000, 1.000000000000000000, 0.000000000000000000 ) ) ;
#14525 = CARTESIAN_POINT ( 'NONE',  ( 158.0000000000000000, 208.4606249624626457, -45.00000000000000000 ) ) ;
#14526 = CARTESIAN_POINT ( 'NONE',  ( 161.2365440327092472, 161.2365440327092472, 45.00000000000000000 ) ) ;
#14527 = ORIENTED_EDGE ( 'NONE', *, *, #25944, .F. ) ;
#14528 = VECTOR ( 'NONE', #3221, 1000.000000000000114 ) ;
#14529 = CARTESIAN_POINT ( 'NONE',  ( -189.6824478863817092, 103.6171365956006980, 32.45239274750386471 ) ) ;
#14530 = EDGE_CURVE ( 'NONE', #21528, #7328, #26897, .T. ) ;
#14531 = CARTESIAN_POINT ( 'NONE',  ( 157.9999999999997442, 251.6023750975910218, 45.00000000000000000 ) ) ;
#14532 = ORIENTED_EDGE ( 'NONE', *, *, #21820, .F. ) ;
#14533 = DIRECTION ( 'NONE',  ( -1.000000000000000000, 0.000000000000000000, 0.000000000000000000 ) ) ;
#14534 = ORIENTED_EDGE ( 'NONE', *, *, #27910, .F. ) ;
#14535 = EDGE_LOOP ( 'NONE', ( #26831, #17664, #16004, #11262 ) ) ;
#14536 = CARTESIAN_POINT ( 'NONE',  ( 114.5273445118512967, 107.2595481030940476, 100.0000000000000142 ) ) ;
#14537 = EDGE_CURVE ( 'NONE', #19657, #9810, #22805, .T. ) ;
#14538 = CARTESIAN_POINT ( 'NONE',  ( 157.9999999999996874, 268.6496251426330559, 45.00000000000000000 ) ) ;
#14539 = ORIENTED_EDGE ( 'NONE', *, *, #13382, .T. ) ;
#14540 = ORIENTED_EDGE ( 'NONE', *, *, #25436, .T. ) ;
#14541 = CARTESIAN_POINT ( 'NONE',  ( 157.4999999999998579, 198.6830624361901414, -45.00000000000000000 ) ) ;
#14542 = DIRECTION ( 'NONE',  ( -0.000000000000000000, -0.000000000000000000, -1.000000000000000000 ) ) ;
#14543 = PLANE ( 'NONE',  #12757 ) ;
#14544 = ORIENTED_EDGE ( 'NONE', *, *, #11212, .F. ) ;
#14545 = EDGE_CURVE ( 'NONE', #25901, #6225, #2092, .T. ) ;
#14546 = CARTESIAN_POINT ( 'NONE',  ( 116.3389527601132869, 113.0483370489294543, 100.0000000000000142 ) ) ;
#14547 = EDGE_LOOP ( 'NONE', ( #25451, #4879, #829, #6490 ) ) ;
#14548 = VECTOR ( 'NONE', #27585, 1000.000000000000227 ) ;
#14549 = CYLINDRICAL_SURFACE ( 'NONE', #3831, 5.999999999999977796 ) ;
#14550 = EDGE_CURVE ( 'NONE', #11738, #6712, #27262, .T. ) ;
#14551 = AXIS2_PLACEMENT_3D ( 'NONE', #15935, #20370, #1674 ) ;
#14552 = ADVANCED_FACE ( 'NONE', ( #25112 ), #20805, .F. ) ;
#14553 = DIRECTION ( 'NONE',  ( 0.8916010070293783896, -0.4528218681382319422, 0.000000000000000000 ) ) ;
#14554 = DIRECTION ( 'NONE',  ( 0.000000000000000000, 0.000000000000000000, -1.000000000000000000 ) ) ;
#14555 = CARTESIAN_POINT ( 'NONE',  ( 158.0000000000009663, 115.6692496847042264, 45.00000000000000000 ) ) ;
#14556 = PLANE ( 'NONE',  #15972 ) ;
#14557 = DIRECTION ( 'NONE',  ( -0.000000000000000000, -0.000000000000000000, -1.000000000000000000 ) ) ;
#14558 = CARTESIAN_POINT ( 'NONE',  ( 163.3295226458395462, 210.1286235168210510, -142.8785553633037182 ) ) ;
#14559 = ORIENTED_EDGE ( 'NONE', *, *, #15165, .F. ) ;
#14560 = DIRECTION ( 'NONE',  ( -0.000000000000000000, 1.000000000000000000, -1.387778780781445429E-16 ) ) ;
#14561 = DIRECTION ( 'NONE',  ( 1.000000000000000000, 0.000000000000000000, -0.000000000000000000 ) ) ;
#14562 = DIRECTION ( 'NONE',  ( 0.4999999999999985012, 0.8660254037844394848, 0.000000000000000000 ) ) ;
#14563 = VERTEX_POINT ( 'NONE', #22827 ) ;
#14564 = LINE ( 'NONE', #25602, #20601 ) ;
#14565 = ORIENTED_EDGE ( 'NONE', *, *, #15870, .F. ) ;
#14566 = DIRECTION ( 'NONE',  ( -0.000000000000000000, -0.000000000000000000, -1.000000000000000000 ) ) ;
#14567 = CARTESIAN_POINT ( 'NONE',  ( 89.99999999999994316, -90.00000000000001421, -25.00000000000000711 ) ) ;
#14568 = LINE ( 'NONE', #18455, #27290 ) ;
#14569 = VERTEX_POINT ( 'NONE', #5429 ) ;
#14570 = LINE ( 'NONE', #1348, #28044 ) ;
#14571 = CARTESIAN_POINT ( 'NONE',  ( 367.9108539694884144, 44.41075299063183479, 100.0000000000000284 ) ) ;
#14572 = ORIENTED_EDGE ( 'NONE', *, *, #19305, .F. ) ;
#14573 = AXIS2_PLACEMENT_3D ( 'NONE', #7012, #18227, #2982 ) ;
#14574 = CARTESIAN_POINT ( 'NONE',  ( 157.9999999999998010, 231.5393750375350237, 45.00000000000000000 ) ) ;
#14575 = CARTESIAN_POINT ( 'NONE',  ( 157.9999999999997158, 263.6338751276190351, -45.00000000000000000 ) ) ;
#14576 = ORIENTED_EDGE ( 'NONE', *, *, #10005, .F. ) ;
#14577 = ORIENTED_EDGE ( 'NONE', *, *, #13285, .T. ) ;
#14578 = DIRECTION ( 'NONE',  ( -1.000000000000000000, 0.000000000000000000, -0.000000000000000000 ) ) ;
#14579 = EDGE_CURVE ( 'NONE', #22232, #3081, #27393, .T. ) ;
#14580 = VERTEX_POINT ( 'NONE', #3266 ) ;
#14581 = EDGE_CURVE ( 'NONE', #26741, #28280, #27552, .T. ) ;
#14582 = ORIENTED_EDGE ( 'NONE', *, *, #27850, .T. ) ;
#14583 = ORIENTED_EDGE ( 'NONE', *, *, #10364, .T. ) ;
#14584 = LINE ( 'NONE', #6091, #28106 ) ;
#14585 = VECTOR ( 'NONE', #16259, 1000.000000000000000 ) ;
#14586 = EDGE_CURVE ( 'NONE', #2819, #25689, #10175, .T. ) ;
#14587 = DIRECTION ( 'NONE',  ( -1.321694076934710155E-16, 1.000000000000000000, 0.000000000000000000 ) ) ;
#14588 = CARTESIAN_POINT ( 'NONE',  ( 158.0000000000006821, 140.7479997597746433, -45.00000000000000000 ) ) ;
#14589 = DIRECTION ( 'NONE',  ( 0.000000000000000000, -1.000000000000000000, 0.000000000000000000 ) ) ;
#14590 = DIRECTION ( 'NONE',  ( 0.8916010070293584056, -0.4528218681382712996, 0.000000000000000000 ) ) ;
#14591 = CARTESIAN_POINT ( 'NONE',  ( -226.8880901706862971, 73.06320664976456669, -17.43415524067905409 ) ) ;
#14592 = EDGE_CURVE ( 'NONE', #8019, #18668, #27955, .T. ) ;
#14593 = CARTESIAN_POINT ( 'NONE',  ( 158.0000000000008811, 121.1928747072253572, 45.00000000000000000 ) ) ;
#14594 = PLANE ( 'NONE',  #3259 ) ;
#14595 = LINE ( 'NONE', #21191, #9586 ) ;
#14596 = CARTESIAN_POINT ( 'NONE',  ( -175.0000000000000000, -150.0000000000000853, 70.00000000000001421 ) ) ;
#14597 = VERTEX_POINT ( 'NONE', #10743 ) ;
#14598 = PLANE ( 'NONE',  #25613 ) ;
#14599 = CARTESIAN_POINT ( 'NONE',  ( 109.9161154791872690, 257.8825900702938725, -41.33255568694282545 ) ) ;
#14600 = CARTESIAN_POINT ( 'NONE',  ( 217.4999999999996305, 133.0668745871126930, 36.86484227207694886 ) ) ;
#14601 = PRESENTATION_STYLE_ASSIGNMENT (( #20775 ) ) ;
#14602 = DIRECTION ( 'NONE',  ( 0.8916010070296023216, -0.4528218681377911281, 0.000000000000000000 ) ) ;
#14603 = EDGE_LOOP ( 'NONE', ( #2785, #24898, #9805, #4582 ) ) ;
#14604 = VECTOR ( 'NONE', #18096, 1000.000000000000114 ) ;
#14605 = DIRECTION ( 'NONE',  ( -0.000000000000000000, -0.000000000000000000, -1.000000000000000000 ) ) ;
#14606 = VERTEX_POINT ( 'NONE', #3691 ) ;
#14607 = CARTESIAN_POINT ( 'NONE',  ( 158.0000000000012790, 85.57474959461971764, 45.00000000000000000 ) ) ;
#14608 = VECTOR ( 'NONE', #16849, 1000.000000000000000 ) ;
#14609 = ORIENTED_EDGE ( 'NONE', *, *, #3016, .F. ) ;
#14610 = ORIENTED_EDGE ( 'NONE', *, *, #6752, .F. ) ;
#14611 = CARTESIAN_POINT ( 'NONE',  ( -47.63323754515640474, 132.2630729665446836, 15.94942322957973069 ) ) ;
#14612 = ADVANCED_FACE ( 'NONE', ( #16642 ), #23669, .F. ) ;
#14613 = ORIENTED_EDGE ( 'NONE', *, *, #26281, .T. ) ;
#14614 = ORIENTED_EDGE ( 'NONE', *, *, #41, .F. ) ;
#14615 = DIRECTION ( 'NONE',  ( 0.000000000000000000, 0.000000000000000000, -1.000000000000000000 ) ) ;
#14616 = DIRECTION ( 'NONE',  ( 0.8916010070299977830, -0.4528218681370124177, 0.000000000000000000 ) ) ;
#14617 = FACE_OUTER_BOUND ( 'NONE', #22445, .T. ) ;
#14618 = VECTOR ( 'NONE', #24735, 1000.000000000000114 ) ;
#14619 = DIRECTION ( 'NONE',  ( 0.000000000000000000, 0.000000000000000000, -1.000000000000000000 ) ) ;
#14620 = CARTESIAN_POINT ( 'NONE',  ( -272.4516753896481873, -165.0365817940426325, -87.32421121213782556 ) ) ;
#14622 = DIRECTION ( 'NONE',  ( 0.000000000000000000, 0.000000000000000000, -1.000000000000000000 ) ) ;
#14621 = VECTOR ( 'NONE', #28245, 1000.000000000000000 ) ;
#14623 = DIRECTION ( 'NONE',  ( 1.000000000000000000, 1.530283246943720875E-16, -0.000000000000000000 ) ) ;
#14624 = EDGE_CURVE ( 'NONE', #7082, #15954, #5715, .T. ) ;
#14625 = PRODUCT_DEFINITION_SHAPE ( 'NONE', 'NONE',  #6305 ) ;
#14626 = ADVANCED_FACE ( 'NONE', ( #5995 ), #24602, .F. ) ;
#14627 = CARTESIAN_POINT ( 'NONE',  ( 133.4403429179407681, 249.9619548141471057, -139.1927212198768586 ) ) ;
#14628 = AXIS2_PLACEMENT_3D ( 'NONE', #4492, #2339, #21361 ) ;
#14629 = CARTESIAN_POINT ( 'NONE',  ( -230.9590218388320295, 90.04903060735585996, 15.10580296129862177 ) ) ;
#14630 = CARTESIAN_POINT ( 'NONE',  ( -43.02437977270766822, 129.7200458115292747, 16.81627168235289815 ) ) ;
#14631 = LINE ( 'NONE', #14774, #21005 ) ;
#14632 = CARTESIAN_POINT ( 'NONE',  ( 115.5814157129578916, 232.3660254037840502, 45.00000000000000000 ) ) ;
#14633 = ORIENTED_EDGE ( 'NONE', *, *, #20672, .T. ) ;
#14634 = LINE ( 'NONE', #12068, #15120 ) ;
#14635 = CARTESIAN_POINT ( 'NONE',  ( 106.7460014144458569, 209.9136339888866303, -147.6607294899350507 ) ) ;
#14637 = ORIENTED_EDGE ( 'NONE', *, *, #2510, .T. ) ;
#14636 = VERTEX_POINT ( 'NONE', #10452 ) ;
#14638 = ADVANCED_FACE ( 'NONE', ( #19211 ), #8301, .F. ) ;
#14639 = EDGE_CURVE ( 'NONE', #1600, #14154, #12179, .T. ) ;
#14640 = AXIS2_PLACEMENT_3D ( 'NONE', #21158, #3626, #12702 ) ;
#14641 = CARTESIAN_POINT ( 'NONE',  ( 100.3999191023820003, 235.3978472240765711, -22.98606999220681857 ) ) ;
#14642 = ORIENTED_EDGE ( 'NONE', *, *, #26575, .F. ) ;
#14643 = ORIENTED_EDGE ( 'NONE', *, *, #8651, .T. ) ;
#14644 = ORIENTED_EDGE ( 'NONE', *, *, #11095, .T. ) ;
#14645 = AXIS2_PLACEMENT_3D ( 'NONE', #11424, #6948, #16020 ) ;
#14646 = ORIENTED_EDGE ( 'NONE', *, *, #2794, .F. ) ;
#14647 = ADVANCED_FACE ( 'NONE', ( #2102 ), #2382, .F. ) ;
#14648 = ORIENTED_EDGE ( 'NONE', *, *, #16275, .T. ) ;
#14649 = ORIENTED_EDGE ( 'NONE', *, *, #11782, .F. ) ;
#14650 = CARTESIAN_POINT ( 'NONE',  ( 158.0000000000002842, 180.8739998798873501, -45.00000000000000000 ) ) ;
#14651 = FACE_OUTER_BOUND ( 'NONE', #24603, .T. ) ;
#14652 = CARTESIAN_POINT ( 'NONE',  ( -270.1025481742786951, -91.18033988749901653, 0.000000000000000000 ) ) ;
#14653 = DIRECTION ( 'NONE',  ( 0.8916010070296327417, 0.4528218681377311206, 0.000000000000000000 ) ) ;
#14654 = CIRCLE ( 'NONE', #4528, 49.99999999999998579 ) ;
#14655 = AXIS2_PLACEMENT_3D ( 'NONE', #11699, #2621, #16143 ) ;
#14656 = CARTESIAN_POINT ( 'NONE',  ( -17.24491960465745777, 0.000000000000000000, 100.0000000000000000 ) ) ;
#14657 = CARTESIAN_POINT ( 'NONE',  ( 1.982541115402066017E-14, -150.0000000000000568, -99.99999999999995737 ) ) ;
#14658 = CARTESIAN_POINT ( 'NONE',  ( -0.000000000000000000, 196.9999999999997442, -45.00000000000000000 ) ) ;
#14659 = AXIS2_PLACEMENT_3D ( 'NONE', #18099, #20388, #9485 ) ;
#14660 = PLANE ( 'NONE',  #8187 ) ;
#14661 = LINE ( 'NONE', #12379, #4065 ) ;
#14662 = LINE ( 'NONE', #19107, #25277 ) ;
#14663 = DIRECTION ( 'NONE',  ( 0.8916010070298151513, -0.4528218681373720744, 0.000000000000000000 ) ) ;
#14664 = VERTEX_POINT ( 'NONE', #2240 ) ;
#14665 = CARTESIAN_POINT ( 'NONE',  ( 157.4999999999998579, 133.4783122410070462, 45.00000000000000000 ) ) ;
#14666 = AXIS2_PLACEMENT_3D ( 'NONE', #14806, #13210, #17785 ) ;
#14667 = CARTESIAN_POINT ( 'NONE',  ( -279.1278187736259611, -170.0000000000001137, -106.1966075482098262 ) ) ;
#14668 = ORIENTED_EDGE ( 'NONE', *, *, #14517, .T. ) ;
#14669 = DIRECTION ( 'NONE',  ( 0.000000000000000000, 0.000000000000000000, 1.000000000000000000 ) ) ;
#14670 = ORIENTED_EDGE ( 'NONE', *, *, #3517, .F. ) ;
#14671 = EDGE_CURVE ( 'NONE', #2370, #4186, #26092, .T. ) ;
#14673 = EDGE_CURVE ( 'NONE', #12815, #19423, #17760, .T. ) ;
#14672 = ORIENTED_EDGE ( 'NONE', *, *, #22006, .T. ) ;
#14674 = DIRECTION ( 'NONE',  ( -0.8916010070298759915, 0.4528218681372521703, 0.000000000000000000 ) ) ;
#14675 = CIRCLE ( 'NONE', #8233, 6.000000000000005329 ) ;
#14676 = DIRECTION ( 'NONE',  ( -0.000000000000000000, 1.000000000000000000, -1.387778780781445429E-16 ) ) ;
#14677 = ORIENTED_EDGE ( 'NONE', *, *, #27938, .F. ) ;
#14678 = ADVANCED_FACE ( 'NONE', ( #22217 ), #6701, .F. ) ;
#14679 = ORIENTED_EDGE ( 'NONE', *, *, #13599, .T. ) ;
#14680 = DIRECTION ( 'NONE',  ( -0.8916010070299477119, -0.4528218681371110610, 0.000000000000000000 ) ) ;
#14681 = CIRCLE ( 'NONE', #5957, 7.499999999999992895 ) ;
#14682 = CARTESIAN_POINT ( 'NONE',  ( 79.99999999999992895, 110.0000000000000000, 70.00000000000001421 ) ) ;
#14683 = AXIS2_PLACEMENT_3D ( 'NONE', #16525, #870, #7758 ) ;
#14684 = CARTESIAN_POINT ( 'NONE',  ( -184.1653517315182569, 107.3698090412221404, -31.09403837874923582 ) ) ;
#14685 = ORIENTED_EDGE ( 'NONE', *, *, #19597, .F. ) ;
#14686 = DIRECTION ( 'NONE',  ( 1.000000000000000000, -0.000000000000000000, -0.000000000000000000 ) ) ;
#14687 = ORIENTED_EDGE ( 'NONE', *, *, #16207, .T. ) ;
#14688 = DIRECTION ( 'NONE',  ( 0.000000000000000000, 0.000000000000000000, -1.000000000000000000 ) ) ;
#14689 = FACE_OUTER_BOUND ( 'NONE', #21695, .T. ) ;
#14690 = CARTESIAN_POINT ( 'NONE',  ( 232.4749999999995964, 83.06687458711267880, -42.86484227207692754 ) ) ;
#14691 = DIRECTION ( 'NONE',  ( -1.321694076934710155E-16, 1.000000000000000000, 0.000000000000000000 ) ) ;
#14692 = LINE ( 'NONE', #10098, #7755 ) ;
#14693 = DIRECTION ( 'NONE',  ( -0.000000000000000000, 0.000000000000000000, -1.000000000000000000 ) ) ;
#14694 = CARTESIAN_POINT ( 'NONE',  ( -192.2868888506042708, 101.5231402318620582, -32.81226276753037041 ) ) ;
#14695 = ORIENTED_EDGE ( 'NONE', *, *, #14838, .F. ) ;
#14696 = VECTOR ( 'NONE', #15340, 1000.000000000000000 ) ;
#14697 = EDGE_CURVE ( 'NONE', #9432, #16411, #19772, .T. ) ;
#14698 = CARTESIAN_POINT ( 'NONE',  ( -41.54405845664282282, 46.26118624020713099, 45.00000000000000000 ) ) ;
#14699 = CARTESIAN_POINT ( 'NONE',  ( -160.0000000000000284, 59.99999999999994316, -15.00000000000000000 ) ) ;
#14700 = DIRECTION ( 'NONE',  ( -0.000000000000000000, 0.000000000000000000, -1.000000000000000000 ) ) ;
#14701 = LINE ( 'NONE', #10813, #24974 ) ;
#14702 = ORIENTED_EDGE ( 'NONE', *, *, #735, .F. ) ;
#14703 = CARTESIAN_POINT ( 'NONE',  ( 117.2367070128591990, 233.8218819039115886, 99.61792820886471134 ) ) ;
#14704 = VECTOR ( 'NONE', #926, 1000.000000000000114 ) ;
#14705 = VERTEX_POINT ( 'NONE', #15198 ) ;
#14706 = CARTESIAN_POINT ( 'NONE',  ( -170.0252337835103162, 115.7161349404674411, 25.41356568217192802 ) ) ;
#14707 = DIRECTION ( 'NONE',  ( 1.000000000000000000, 0.000000000000000000, -0.000000000000000000 ) ) ;
#14708 = CARTESIAN_POINT ( 'NONE',  ( -205.2925087133504860, 91.43105200015486389, 27.40227028352467897 ) ) ;
#14709 = VERTEX_POINT ( 'NONE', #247 ) ;
#14710 = LINE ( 'NONE', #10120, #77 ) ;
#14711 = DIRECTION ( 'NONE',  ( -0.000000000000000000, -0.000000000000000000, -1.000000000000000000 ) ) ;
#14712 = ADVANCED_FACE ( 'NONE', ( #21797 ), #26510, .T. ) ;
#14713 = ORIENTED_EDGE ( 'NONE', *, *, #13484, .T. ) ;
#14714 = EDGE_CURVE ( 'NONE', #7154, #25274, #8721, .T. ) ;
#14715 = EDGE_CURVE ( 'NONE', #17607, #23614, #24155, .T. ) ;
#14716 = LINE ( 'NONE', #15001, #1906 ) ;
#14717 = ADVANCED_FACE ( 'NONE', ( #2670 ), #3509, .F. ) ;
#14718 = LINE ( 'NONE', #23469, #3015 ) ;
#14719 = VERTEX_POINT ( 'NONE', #21931 ) ;
#14720 = ORIENTED_EDGE ( 'NONE', *, *, #21599, .T. ) ;
#14721 = CARTESIAN_POINT ( 'NONE',  ( 158.0000000000011653, 93.60624962464788723, -45.00000000000000000 ) ) ;
#14722 = VERTEX_POINT ( 'NONE', #11313 ) ;
#14723 = VECTOR ( 'NONE', #25498, 1000.000000000000000 ) ;
#14724 = ORIENTED_EDGE ( 'NONE', *, *, #25843, .F. ) ;
#14725 = VERTEX_POINT ( 'NONE', #15771 ) ;
#14726 = CARTESIAN_POINT ( 'NONE',  ( 158.0000000000013074, 83.06687458711267880, 45.00000000000000000 ) ) ;
#14727 = AXIS2_PLACEMENT_3D ( 'NONE', #13058, #24235, #13332 ) ;
#14728 = DIRECTION ( 'NONE',  ( -0.000000000000000000, -0.000000000000000000, -1.000000000000000000 ) ) ;
#14729 = CARTESIAN_POINT ( 'NONE',  ( -68.57415822541635464, 24.64876300893806160, 95.00000000000000000 ) ) ;
#14730 = CARTESIAN_POINT ( 'NONE',  ( 157.4999999999998579, 161.0649373235845019, -45.00000000000000000 ) ) ;
#14731 = CARTESIAN_POINT ( 'NONE',  ( 89.99999999999994316, -70.00000000000001421, -70.00000000000001421 ) ) ;
#14732 = DIRECTION ( 'NONE',  ( 0.000000000000000000, 0.000000000000000000, 1.000000000000000000 ) ) ;
#14733 = CARTESIAN_POINT ( 'NONE',  ( -244.5479615644635487, 75.99513337129094737, -5.000000000000002665 ) ) ;
#14734 = ORIENTED_EDGE ( 'NONE', *, *, #20379, .F. ) ;
#14735 = FACE_OUTER_BOUND ( 'NONE', #3064, .T. ) ;
#14736 = CARTESIAN_POINT ( 'NONE',  ( 157.4999999999998579, 221.2539375037535194, 45.00000000000000000 ) ) ;
#14737 = DIRECTION ( 'NONE',  ( 0.000000000000000000, 0.000000000000000000, 1.000000000000000000 ) ) ;
#14738 = CARTESIAN_POINT ( 'NONE',  ( 115.6411010564591777, 231.4666050640012429, -99.00000000000001421 ) ) ;
#14739 = ORIENTED_EDGE ( 'NONE', *, *, #27962, .T. ) ;
#14740 = PLANE ( 'NONE',  #9117 ) ;
#14741 = EDGE_CURVE ( 'NONE', #8883, #3705, #2522, .T. ) ;
#14742 = EDGE_CURVE ( 'NONE', #13433, #8883, #26657, .T. ) ;
#14743 =( GEOMETRIC_REPRESENTATION_CONTEXT ( 3 ) GLOBAL_UNCERTAINTY_ASSIGNED_CONTEXT ( ( #13211 ) ) GLOBAL_UNIT_ASSIGNED_CONTEXT ( ( #10035, #22965, #5153 ) ) REPRESENTATION_CONTEXT ( 'NONE', 'WORKASPACE' ) );
#14744 = FACE_OUTER_BOUND ( 'NONE', #25653, .T. ) ;
#14745 = PLANE ( 'NONE',  #17216 ) ;
#14746 = CARTESIAN_POINT ( 'NONE',  ( -260.0000000000001137, -152.0000000000000284, -104.9999999999998721 ) ) ;
#14747 = DIRECTION ( 'NONE',  ( -0.8916010070293383105, -0.4528218681383106015, 0.000000000000000000 ) ) ;
#14748 = ORIENTED_EDGE ( 'NONE', *, *, #10910, .F. ) ;
#14749 = EDGE_CURVE ( 'NONE', #27317, #21276, #15343, .T. ) ;
#14750 = VECTOR ( 'NONE', #19538, 1000.000000000000000 ) ;
#14751 = DIRECTION ( 'NONE',  ( 0.000000000000000000, 1.000000000000000000, 0.000000000000000000 ) ) ;
#14752 = ORIENTED_EDGE ( 'NONE', *, *, #28046, .F. ) ;
#14753 = ADVANCED_FACE ( 'NONE', ( #17334 ), #4401, .F. ) ;
#14754 = DIRECTION ( 'NONE',  ( 0.8916010070299369428, -0.4528218681371322663, 0.000000000000000000 ) ) ;
#14755 = VERTEX_POINT ( 'NONE', #24945 ) ;
#14756 = VERTEX_POINT ( 'NONE', #27362 ) ;
#14757 = DIRECTION ( 'NONE',  ( 0.000000000000000000, 0.000000000000000000, 1.000000000000000000 ) ) ;
#14758 = EDGE_LOOP ( 'NONE', ( #6291, #2544, #6218, #8072 ) ) ;
#14759 = VERTEX_POINT ( 'NONE', #24805 ) ;
#14760 = CARTESIAN_POINT ( 'NONE',  ( 112.7775258882239910, 216.4408397934976449, 96.91707758366527514 ) ) ;
#14761 = CARTESIAN_POINT ( 'NONE',  ( 158.0000000000005116, 158.8109998198309825, -45.00000000000000000 ) ) ;
#14762 = DIRECTION ( 'NONE',  ( 0.4528218681377710886, 0.8916010070296124246, -0.000000000000000000 ) ) ;
#14763 = VECTOR ( 'NONE', #2242, 1000.000000000000000 ) ;
#14764 = CARTESIAN_POINT ( 'NONE',  ( -152.9413447092802869, 123.6266336979618785, -18.69402831667922626 ) ) ;
#14765 = CIRCLE ( 'NONE', #20253, 50.00000000000000000 ) ;
#14766 = VECTOR ( 'NONE', #25120, 1000.000000000000000 ) ;
#14767 = CARTESIAN_POINT ( 'NONE',  ( -269.2930304670530290, -170.4418591343095386, -88.55248351026435216 ) ) ;
#14768 = CARTESIAN_POINT ( 'NONE',  ( -260.0000000000001137, -167.0819201924624906, 110.0000000000000142 ) ) ;
#14769 = CARTESIAN_POINT ( 'NONE',  ( 29.75659119584032908, -42.58214737927222160, 99.89076439235542182 ) ) ;
#14770 = CARTESIAN_POINT ( 'NONE',  ( -218.9419962481124742, 86.22404402610023055, -19.29714585459672094 ) ) ;
#14771 = DIRECTION ( 'NONE',  ( 1.000000000000000000, -0.000000000000000000, -0.000000000000000000 ) ) ;
#14772 = PLANE ( 'NONE',  #28199 ) ;
#14773 = DIRECTION ( 'NONE',  ( 3.053113317719176147E-15, 4.035281788239917819E-31, 1.000000000000000000 ) ) ;
#14774 = CARTESIAN_POINT ( 'NONE',  ( 158.0000000000017337, 42.94087446699998623, -45.00000000000000000 ) ) ;
#14775 = CARTESIAN_POINT ( 'NONE',  ( 157.4999999999998295, 231.2854375337815327, 45.00000000000000000 ) ) ;
#14776 = VERTEX_POINT ( 'NONE', #22795 ) ;
#14777 = EDGE_CURVE ( 'NONE', #13271, #21857, #4966, .T. ) ;
#14778 = LINE ( 'NONE', #25680, #16496 ) ;
#14779 = CARTESIAN_POINT ( 'NONE',  ( -71.37541315349507443, 150.2892445414773590, 15.00000000000000000 ) ) ;
#14780 = FACE_OUTER_BOUND ( 'NONE', #2753, .T. ) ;
#14782 = ORIENTED_EDGE ( 'NONE', *, *, #17402, .T. ) ;
#14781 = ORIENTED_EDGE ( 'NONE', *, *, #25482, .T. ) ;
#14783 = AXIS2_PLACEMENT_3D ( 'NONE', #23598, #10248, #21434 ) ;
#14784 = CARTESIAN_POINT ( 'NONE',  ( 96.75280658369999287, 240.7143248587423159, -19.91790936281032032 ) ) ;
#14785 = ORIENTED_EDGE ( 'NONE', *, *, #3021, .T. ) ;
#14786 = ORIENTED_EDGE ( 'NONE', *, *, #5201, .F. ) ;
#14787 = VECTOR ( 'NONE', #10962, 1000.000000000000114 ) ;
#14788 =( GEOMETRIC_REPRESENTATION_CONTEXT ( 3 ) GLOBAL_UNCERTAINTY_ASSIGNED_CONTEXT ( ( #7454 ) ) GLOBAL_UNIT_ASSIGNED_CONTEXT ( ( #5896, #25297, #18557 ) ) REPRESENTATION_CONTEXT ( 'NONE', 'WORKASPACE' ) );
#14789 = ORIENTED_EDGE ( 'NONE', *, *, #27927, .T. ) ;
#14790=STYLED_ITEM('',(#28427),#8903);
#14791 = EDGE_CURVE ( 'NONE', #7370, #24416, #6711, .T. ) ;
#14792 = EDGE_LOOP ( 'NONE', ( #20265, #25743, #25519, #21522 ) ) ;
#14793 = ORIENTED_EDGE ( 'NONE', *, *, #6294, .F. ) ;
#14794 = ORIENTED_EDGE ( 'NONE', *, *, #18841, .T. ) ;
#14795 = LINE ( 'NONE', #1987, #13203 ) ;
#14796 = DIRECTION ( 'NONE',  ( 0.000000000000000000, 0.000000000000000000, -1.000000000000000000 ) ) ;
#14797 = DIRECTION ( 'NONE',  ( 0.000000000000000000, 2.498359269027536814E-16, -1.000000000000000000 ) ) ;
#14798 = ADVANCED_FACE ( 'NONE', ( #22654 ), #15914, .T. ) ;
#14799 = VECTOR ( 'NONE', #25078, 1000.000000000000000 ) ;
#14800 = CARTESIAN_POINT ( 'NONE',  ( -17.95129507155921544, 128.7178007427875457, -17.19838318425743040 ) ) ;
#14801 = EDGE_CURVE ( 'NONE', #20650, #25890, #14177, .T. ) ;
#14802 = AXIS2_PLACEMENT_3D ( 'NONE', #2174, #6347, #4465 ) ;
#14803 = APPLICATION_CONTEXT ( 'automotive_design' ) ;
#14804 = DIRECTION ( 'NONE',  ( -0.000000000000000000, 0.2756732917354685064, -0.9612513907525602752 ) ) ;
#14805 = CARTESIAN_POINT ( 'NONE',  ( -63.57415822541634043, -18.01420295945611727, 95.00000000000000000 ) ) ;
#14806 = CARTESIAN_POINT ( 'NONE',  ( 157.4999999999998579, 151.0334372935563465, 45.00000000000000000 ) ) ;
#14807 = CARTESIAN_POINT ( 'NONE',  ( -208.5031313904178774, 74.88898109331546493, -38.37316925720519833 ) ) ;
#14808 = AXIS2_PLACEMENT_3D ( 'NONE', #7331, #11510, #581 ) ;
#14809 = EDGE_CURVE ( 'NONE', #16142, #14865, #14045, .T. ) ;
#14810 = CARTESIAN_POINT ( 'NONE',  ( 112.5440210185366681, 200.1070613527027433, -144.6008566625276330 ) ) ;
#14811 = DIRECTION ( 'NONE',  ( -1.000000000000000000, 0.000000000000000000, 0.000000000000000000 ) ) ;
#14812 = DIRECTION ( 'NONE',  ( 0.000000000000000000, -1.000000000000000000, -1.214306433183764966E-16 ) ) ;
#14813 = DIRECTION ( 'NONE',  ( 0.7071067811865474617, -0.7071067811865474617, 0.000000000000000000 ) ) ;
#14814 = ORIENTED_EDGE ( 'NONE', *, *, #15507, .F. ) ;
#14815 = CARTESIAN_POINT ( 'NONE',  ( 115.6411010564591777, 231.4666050640012429, -99.00000000000001421 ) ) ;
#14816 = DIRECTION ( 'NONE',  ( 1.000000000000000000, -0.000000000000000000, -0.000000000000000000 ) ) ;
#14817 = ORIENTED_EDGE ( 'NONE', *, *, #2472, .F. ) ;
#14818 = CONTEXT_DEPENDENT_SHAPE_REPRESENTATION ( #4496, #10970 ) ;
#14819 = EDGE_LOOP ( 'NONE', ( #1108, #15151, #21581, #24492 ) ) ;
#14820 = VECTOR ( 'NONE', #2769, 1000.000000000000000 ) ;
#14821 = ORIENTED_EDGE ( 'NONE', *, *, #3005, .T. ) ;
#14822 = EDGE_CURVE ( 'NONE', #17042, #1725, #9443, .T. ) ;
#14823 = ADVANCED_FACE ( 'NONE', ( #950 ), #20768, .F. ) ;
#14824 = AXIS2_PLACEMENT_3D ( 'NONE', #13227, #6605, #17662 ) ;
#14825 = DIRECTION ( 'NONE',  ( 0.4528218681383106015, -0.8916010070293384215, 0.000000000000000000 ) ) ;
#14826 = CARTESIAN_POINT ( 'NONE',  ( -125.2895325436292069, 200.2180533211636657, 15.00000000000000000 ) ) ;
#14827 = ORIENTED_EDGE ( 'NONE', *, *, #16661, .T. ) ;
#14828 = VECTOR ( 'NONE', #13504, 1000.000000000000000 ) ;
#14829 = ORIENTED_EDGE ( 'NONE', *, *, #22761, .F. ) ;
#14830 = DIRECTION ( 'NONE',  ( 0.4528218681383106015, -0.8916010070293384215, 0.000000000000000000 ) ) ;
#14831 = AXIS2_PLACEMENT_3D ( 'NONE', #4660, #8984, #80 ) ;
#14832 = CARTESIAN_POINT ( 'NONE',  ( 105.5625267348463581, 242.0882338934268887, 29.27839960683066067 ) ) ;
#14833 = CARTESIAN_POINT ( 'NONE',  ( -188.7053934046000734, 104.3037723739169991, -31.95410354694828925 ) ) ;
#14834 = ORIENTED_EDGE ( 'NONE', *, *, #13982, .T. ) ;
#14835 = CARTESIAN_POINT ( 'NONE',  ( 99.60675733924549036, 85.63108538499666622, 100.0000000000000142 ) ) ;
#14836 = ORIENTED_EDGE ( 'NONE', *, *, #1009, .F. ) ;
#14837 = CARTESIAN_POINT ( 'NONE',  ( -248.1546605714623013, -91.18033988749901653, -10.70611877156249214 ) ) ;
#14838 = EDGE_CURVE ( 'NONE', #23257, #19128, #9719, .T. ) ;
#14839 = FACE_OUTER_BOUND ( 'NONE', #13888, .T. ) ;
#14840 = LINE ( 'NONE', #3758, #15039 ) ;
#14841 = EDGE_CURVE ( 'NONE', #10216, #16435, #7570, .T. ) ;
#14842 = VECTOR ( 'NONE', #24320, 1000.000000000000000 ) ;
#14843 = EDGE_CURVE ( 'NONE', #25070, #16727, #26915, .T. ) ;
#14844 = CARTESIAN_POINT ( 'NONE',  ( 111.9999999999999289, 218.9999999999996874, 45.00000000000000000 ) ) ;
#14845 = CARTESIAN_POINT ( 'NONE',  ( 163.4430707983499076, 210.4607210870969709, -144.2074248490018249 ) ) ;
#14846 = ORIENTED_EDGE ( 'NONE', *, *, #23003, .F. ) ;
#14847 = VECTOR ( 'NONE', #14151, 1000.000000000000114 ) ;
#14848 = CARTESIAN_POINT ( 'NONE',  ( 158.0000000000003695, 171.3503748573662051, -45.00000000000000000 ) ) ;
#14849 = EDGE_CURVE ( 'NONE', #17961, #24788, #18481, .T. ) ;
#14850 = FACE_OUTER_BOUND ( 'NONE', #27381, .T. ) ;
#14851 = DIRECTION ( 'NONE',  ( 0.000000000000000000, 0.000000000000000000, -1.000000000000000000 ) ) ;
#14852 = VECTOR ( 'NONE', #25505, 1000.000000000000000 ) ;
#14853 = LINE ( 'NONE', #5927, #26798 ) ;
#14854 = ORIENTED_EDGE ( 'NONE', *, *, #12953, .T. ) ;
#14855 = DIRECTION ( 'NONE',  ( 3.469446951953614189E-16, -1.000000000000000000, 0.000000000000000000 ) ) ;
#14856 = DIRECTION ( 'NONE',  ( 1.000000000000000000, 0.000000000000000000, 0.000000000000000000 ) ) ;
#14857 = FACE_OUTER_BOUND ( 'NONE', #17527, .T. ) ;
#14858 = CARTESIAN_POINT ( 'NONE',  ( 158.0000000000012506, 86.08262460212675649, 45.00000000000000000 ) ) ;
#14859 = ORIENTED_EDGE ( 'NONE', *, *, #16178, .T. ) ;
#14860 = DIRECTION ( 'NONE',  ( 1.000000000000000000, 0.000000000000000000, 0.000000000000000000 ) ) ;
#14861 = CYLINDRICAL_SURFACE ( 'NONE', #15264, 30.00000000000000000 ) ;
#14862 = VERTEX_POINT ( 'NONE', #679 ) ;
#14863 = DIRECTION ( 'NONE',  ( -0.000000000000000000, 1.000000000000000000, -1.387778780781445429E-16 ) ) ;
#14864 = CARTESIAN_POINT ( 'NONE',  ( -199.1750262236165270, 96.10583454779617796, -31.38733092741667008 ) ) ;
#14865 = VERTEX_POINT ( 'NONE', #18058 ) ;
#14866 = EDGE_CURVE ( 'NONE', #16038, #19152, #1089, .T. ) ;
#14867 = VECTOR ( 'NONE', #22573, 1000.000000000000227 ) ;
#14868 = ORIENTED_EDGE ( 'NONE', *, *, #26220, .F. ) ;
#14869 = CARTESIAN_POINT ( 'NONE',  ( -210.0000000000000000, -218.4793454996983826, -109.3807997302051973 ) ) ;
#14870 = ORIENTED_EDGE ( 'NONE', *, *, #13609, .T. ) ;
#14871 = PRODUCT ( 'Structural Component', 'Structural Component', '', ( #24001 ) ) ;
#14872 = ORIENTED_EDGE ( 'NONE', *, *, #1960, .F. ) ;
#14873 = VERTEX_POINT ( 'NONE', #12023 ) ;
#14874 = CARTESIAN_POINT ( 'NONE',  ( 179.9999999999999147, -5.589247009368138563, -84.99999999999997158 ) ) ;
#14875 = CARTESIAN_POINT ( 'NONE',  ( 158.0000000000012221, 88.59049960963380954, -45.00000000000000000 ) ) ;
#14876 = CARTESIAN_POINT ( 'NONE',  ( 6.333040578238042784, 140.1900314533376388, 13.00000000000000355 ) ) ;
#14877 = LINE ( 'NONE', #10136, #3200 ) ;
#14878 = EDGE_CURVE ( 'NONE', #12331, #9062, #16197, .T. ) ;
#14879 = EDGE_CURVE ( 'NONE', #10475, #25995, #21854, .T. ) ;
#14880 = CARTESIAN_POINT ( 'NONE',  ( 157.4999999999998579, 108.3995621659365867, 45.00000000000000000 ) ) ;
#14881 = CARTESIAN_POINT ( 'NONE',  ( 157.4999999999998579, 133.4783122410070462, 45.00000000000000000 ) ) ;
#14882 = CARTESIAN_POINT ( 'NONE',  ( -236.2188936947904381, 81.35702876104954839, -15.00000000000000178 ) ) ;
#14883 = ORIENTED_EDGE ( 'NONE', *, *, #13884, .F. ) ;
#14884 = CARTESIAN_POINT ( 'NONE',  ( 158.0000000000014211, 71.03537455708449500, -45.00000000000000000 ) ) ;
#14885 = DIRECTION ( 'NONE',  ( 0.4528218681382713551, 0.8916010070293584056, -0.000000000000000000 ) ) ;
#14886 = DIRECTION ( 'NONE',  ( 0.000000000000000000, 1.214306433183764720E-16, -1.000000000000000000 ) ) ;
#14887 = CARTESIAN_POINT ( 'NONE',  ( 158.0000000000001705, 188.9054999099155054, -45.00000000000000000 ) ) ;
#14888 = ORIENTED_EDGE ( 'NONE', *, *, #7440, .F. ) ;
#14889 = AXIS2_PLACEMENT_3D ( 'NONE', #4567, #19379, #28130 ) ;
#14890 = DIRECTION ( 'NONE',  ( -0.000000000000000000, -0.000000000000000000, -1.000000000000000000 ) ) ;
#14891 = DIRECTION ( 'NONE',  ( 0.000000000000000000, 0.000000000000000000, -1.000000000000000000 ) ) ;
#14892 = DIRECTION ( 'NONE',  ( 0.000000000000000000, -1.000000000000000000, -1.214306433183764966E-16 ) ) ;
#14893 = DIRECTION ( 'NONE',  ( 0.4528218681383106015, 0.8916010070293384215, -0.000000000000000000 ) ) ;
#14894 = DIRECTION ( 'NONE',  ( 1.000000000000000000, 0.000000000000000000, 0.000000000000000000 ) ) ;
#14895 = CIRCLE ( 'NONE', #21753, 79.71075545852265520 ) ;
#14896 = ORIENTED_EDGE ( 'NONE', *, *, #16697, .F. ) ;
#14897 = CARTESIAN_POINT ( 'NONE',  ( 217.4999999999996305, 83.06687458711267880, 30.86484227207694886 ) ) ;
#14898 = VERTEX_POINT ( 'NONE', #7135 ) ;
#14899 = LINE ( 'NONE', #3958, #14942 ) ;
#14900 = ORIENTED_EDGE ( 'NONE', *, *, #20281, .F. ) ;
#14901 = ORIENTED_EDGE ( 'NONE', *, *, #6756, .F. ) ;
#14902 = CARTESIAN_POINT ( 'NONE',  ( -52.43980137721120371, 133.2615281902219238, 14.19467156484360082 ) ) ;
#14903 = ORIENTED_EDGE ( 'NONE', *, *, #20444, .T. ) ;
#14904 = ORIENTED_EDGE ( 'NONE', *, *, #9189, .F. ) ;
#14905 = DIRECTION ( 'NONE',  ( 0.8916010070296022105, 0.4528218681377911281, 0.000000000000000000 ) ) ;
#14906 = AXIS2_PLACEMENT_3D ( 'NONE', #165, #26162, #2448 ) ;
#14907 = CARTESIAN_POINT ( 'NONE',  ( -175.0000000000000000, -150.0000000000000853, -75.99999999999998579 ) ) ;
#14908 = CARTESIAN_POINT ( 'NONE',  ( -70.31278697424053803, 101.4626071723526195, -145.0000000000000000 ) ) ;
#14909 = CARTESIAN_POINT ( 'NONE',  ( -122.9571926194021501, 132.7586943017250007, -14.33743497904945485 ) ) ;
#14910 = VECTOR ( 'NONE', #1382, 1000.000000000000227 ) ;
#14911 = ADVANCED_FACE ( 'NONE', ( #7281 ), #24661, .F. ) ;
#14912 = CARTESIAN_POINT ( 'NONE',  ( -272.6023736344520785, -170.1165736173990695, -87.25084524916873363 ) ) ;
#14913 = CARTESIAN_POINT ( 'NONE',  ( -261.1919288306252724, -171.9377729149742038, 90.00000000000001421 ) ) ;
#14914 = CARTESIAN_POINT ( 'NONE',  ( -209.6054486774690133, 88.33790154040774212, -25.57920806210336551 ) ) ;
#14915 = EDGE_CURVE ( 'NONE', #19302, #27032, #20489, .T. ) ;
#14916 = CARTESIAN_POINT ( 'NONE',  ( 131.3377705351922202, 249.7774415780391450, -140.2311020877163230 ) ) ;
#14917 = DIRECTION ( 'NONE',  ( -0.8660254037844326014, 0.5000000000000106581, 0.000000000000000000 ) ) ;
#14918 = DIRECTION ( 'NONE',  ( -0.8916010070297142320, -0.4528218681375706933, 0.000000000000000000 ) ) ;
#14919 = CARTESIAN_POINT ( 'NONE',  ( 134.9999999999998579, 467.1080826427131001, -155.7188177565815010 ) ) ;
#14920 = LINE ( 'NONE', #19356, #19408 ) ;
#14921 = ORIENTED_EDGE ( 'NONE', *, *, #13967, .T. ) ;
#14922 = CARTESIAN_POINT ( 'NONE',  ( 113.8545328002507659, 140.0000000000000284, 97.99666842398181643 ) ) ;
#14923 = DIRECTION ( 'NONE',  ( -0.000000000000000000, -0.000000000000000000, -1.000000000000000000 ) ) ;
#14924 = CARTESIAN_POINT ( 'NONE',  ( 134.9999999999998579, 220.0000000000000284, -119.9999999999999858 ) ) ;
#14926 = VERTEX_POINT ( 'NONE', #27092 ) ;
#14925 = ORIENTED_EDGE ( 'NONE', *, *, #3309, .T. ) ;
#14927 = AXIS2_PLACEMENT_3D ( 'NONE', #20201, #20053, #17905 ) ;
#14928 = CIRCLE ( 'NONE', #2513, 22.49999999999997868 ) ;
#14929 = CARTESIAN_POINT ( 'NONE',  ( 98.38712641049866647, 233.7235291372444692, -21.27834768225378426 ) ) ;
#14930 = EDGE_LOOP ( 'NONE', ( #27102, #16826, #18638, #19480 ) ) ;
#14931 = EDGE_LOOP ( 'NONE', ( #19059, #2542, #790, #27378, #10862 ) ) ;
#14932 = VECTOR ( 'NONE', #19148, 1000.000000000000000 ) ;
#14933 = EDGE_LOOP ( 'NONE', ( #26189, #8987, #3592, #20419 ) ) ;
#14934 = VERTEX_POINT ( 'NONE', #7423 ) ;
#14935 = ORIENTED_EDGE ( 'NONE', *, *, #24536, .T. ) ;
#14936 = EDGE_LOOP ( 'NONE', ( #7264, #11071, #9571, #15057 ) ) ;
#14937 = CARTESIAN_POINT ( 'NONE',  ( 147.1752285801744904, 204.1329331941753082, 45.00000000000000000 ) ) ;
#14938 = ADVANCED_FACE ( 'NONE', ( #14735 ), #25364, .F. ) ;
#14939 = DIRECTION ( 'NONE',  ( 0.8916010070293409751, 0.4528218681383056610, 0.000000000000000000 ) ) ;
#14940 = VECTOR ( 'NONE', #13008, 1000.000000000000000 ) ;
#14941 = VECTOR ( 'NONE', #2201, 1000.000000000000000 ) ;
#14942 = VECTOR ( 'NONE', #7998, 1000.000000000000114 ) ;
#14943 = CARTESIAN_POINT ( 'NONE',  ( 106.6902583091410719, 244.3125670946242849, -31.28102666700890211 ) ) ;
#14944 = DIRECTION ( 'NONE',  ( -0.000000000000000000, -0.000000000000000000, -1.000000000000000000 ) ) ;
#14945 = EDGE_CURVE ( 'NONE', #21625, #17150, #1783, .T. ) ;
#14946 = CARTESIAN_POINT ( 'NONE',  ( 158.0000000000014211, 71.03537455708449500, -45.00000000000000000 ) ) ;
#14947 = VECTOR ( 'NONE', #6663, 1000.000000000000000 ) ;
#14948 = CARTESIAN_POINT ( 'NONE',  ( 157.4999999999998579, 198.6830624361901414, -45.00000000000000000 ) ) ;
#14949 = CARTESIAN_POINT ( 'NONE',  ( -227.3081281289699973, 73.26923787007372368, -17.24424915250854085 ) ) ;
#14950 = EDGE_CURVE ( 'NONE', #24050, #10433, #12591, .T. ) ;
#14951 = CARTESIAN_POINT ( 'NONE',  ( -33.92892658514118409, 128.1932174690772683, 17.41923701875080965 ) ) ;
#14952 = CARTESIAN_POINT ( 'NONE',  ( -40.40953891503691153, 0.000000000000000000, 100.0000000000000000 ) ) ;
#14953 = CARTESIAN_POINT ( 'NONE',  ( 157.4999999999998010, 236.3011875487955251, -45.00000000000000000 ) ) ;
#14954 = LINE ( 'NONE', #8190, #19365 ) ;
#14955 = ORIENTED_EDGE ( 'NONE', *, *, #8817, .F. ) ;
#14956 = CARTESIAN_POINT ( 'NONE',  ( -163.7740599641838912, 118.1414984323162258, 24.33163590040494739 ) ) ;
#14957 = DIRECTION ( 'NONE',  ( 0.8916010070296226386, -0.4528218681377511046, 0.000000000000000000 ) ) ;
#14958 = VERTEX_POINT ( 'NONE', #21330 ) ;
#14959 = ITEM_DEFINED_TRANSFORMATION ( 'NONE', 'NONE', #26232,  #10637 ) ;
#14960 = AXIS2_PLACEMENT_3D ( 'NONE', #11492, #10658, #26270 ) ;
#14961 = EDGE_LOOP ( 'NONE', ( #12012, #22880, #7183, #6363, #20145 ) ) ;
#14962 = VECTOR ( 'NONE', #23008, 1000.000000000000114 ) ;
#14963 = ADVANCED_FACE ( 'NONE', ( #16882 ), #14987, .T. ) ;
#14964 = ORIENTED_EDGE ( 'NONE', *, *, #6976, .T. ) ;
#14965 = CARTESIAN_POINT ( 'NONE',  ( 157.4999999999998579, 161.0649373235845019, 45.00000000000000000 ) ) ;
#14966 = DIRECTION ( 'NONE',  ( 1.000000000000000000, 1.321694076934710155E-16, 0.000000000000000000 ) ) ;
#14967 = ORIENTED_EDGE ( 'NONE', *, *, #9659, .T. ) ;
#14968 = VECTOR ( 'NONE', #23026, 999.9999999999998863 ) ;
#14969 = ORIENTED_EDGE ( 'NONE', *, *, #14191, .F. ) ;
#14970 = CARTESIAN_POINT ( 'NONE',  ( 95.20156243613460845, 83.09913198707280912, -100.0000000000000284 ) ) ;
#14971 = ADVANCED_FACE ( 'NONE', ( #3659 ), #27786, .T. ) ;
#14972 = CARTESIAN_POINT ( 'NONE',  ( 65.00000000000000000, -120.0000000000000711, 70.00000000000001421 ) ) ;
#14973 = CARTESIAN_POINT ( 'NONE',  ( 158.0000000000011653, 93.60624962464788723, 45.00000000000000000 ) ) ;
#14974 = ORIENTED_EDGE ( 'NONE', *, *, #23837, .T. ) ;
#14975 = CARTESIAN_POINT ( 'NONE',  ( -213.6112859001962363, 88.11147169443837868, 20.55567103321151734 ) ) ;
#14976 = ORIENTED_EDGE ( 'NONE', *, *, #27994, .F. ) ;
#14977 = DIRECTION ( 'NONE',  ( 0.000000000000000000, 0.000000000000000000, -1.000000000000000000 ) ) ;
#14978 = CARTESIAN_POINT ( 'NONE',  ( 157.4999999999996874, 268.9035626463865469, -45.00000000000000000 ) ) ;
#14979 = DIRECTION ( 'NONE',  ( 0.8916010070295309342, -0.4528218681379315713, 0.000000000000000000 ) ) ;
#14980 = CIRCLE ( 'NONE', #23225, 5.000000000000000000 ) ;
#14981 = CARTESIAN_POINT ( 'NONE',  ( 158.0000000000006537, 145.7637497747887210, 45.00000000000000000 ) ) ;
#14982 = B_SPLINE_CURVE_WITH_KNOTS ( 'NONE', 3,
 ( #9477, #24978, #22825, #26981, #11640, #20803, #16640, #9890, #2990, #27125, #5427, #3125, #18372, #20521, #2848, #980, #27259, #10031, #25253, #14212, #11781, #7458, #24839, #11919, #25395, #20941, #22960, #7734 ),
 .UNSPECIFIED., .F., .F.,
 ( 4, 2, 2, 2, 2, 2, 2, 2, 2, 2, 2, 2, 2, 4 ),
 ( 0.000000000000000000, 0.01515445388940273724, 0.03030890777880547449, 0.04546336166820825336, 0.05304058861290963933, 0.05682920208526034273, 0.06061781555761103224, 0.07577226944701370703, 0.09092672333641636795, 0.09850395028111769147, 0.1060811772258190289, 0.1098697906981696837, 0.1136584041705203107, 0.1212356311152215788 ),
 .UNSPECIFIED. ) ;
#14983 = ORIENTED_EDGE ( 'NONE', *, *, #23454, .T. ) ;
#14984 = EDGE_CURVE ( 'NONE', #1752, #15077, #2586, .T. ) ;
#14985 = EDGE_CURVE ( 'NONE', #14089, #3705, #1511, .T. ) ;
#14986 = PLANE ( 'NONE',  #18719 ) ;
#14988 = CARTESIAN_POINT ( 'NONE',  ( 232.4999999999996305, 83.06687458711267880, -30.86484227207694886 ) ) ;
#14987 = TOROIDAL_SURFACE ( 'NONE', #9480, 18.46313063346208239, 2.000000000000000000 ) ;
#14989 = DIRECTION ( 'NONE',  ( 0.000000000000000000, -1.000000000000000000, -0.000000000000000000 ) ) ;
#14990 = CARTESIAN_POINT ( 'NONE',  ( 217.4999999999996305, 83.06687458711267880, -30.86484227207694886 ) ) ;
#14991 = ORIENTED_EDGE ( 'NONE', *, *, #5580, .F. ) ;
#14992 = CARTESIAN_POINT ( 'NONE',  ( 122.8247714198253959, 235.8670668058242939, 45.00000000000000000 ) ) ;
#14993 = CARTESIAN_POINT ( 'NONE',  ( -188.8008884155350131, 104.2369363794606443, 31.96258592612735683 ) ) ;
#14994 = CARTESIAN_POINT ( 'NONE',  ( 49.56615429303207065, 203.2034914284457159, -13.00000000000000000 ) ) ;
#14995 = DIRECTION ( 'NONE',  ( 1.000000000000000000, 0.000000000000000000, -0.000000000000000000 ) ) ;
#14996 = EDGE_LOOP ( 'NONE', ( #9876, #4244, #12976, #12603 ) ) ;
#14997 = CARTESIAN_POINT ( 'NONE',  ( 217.4999999999996305, 494.4107529906318632, -100.0000000000000142 ) ) ;
#14998 = ORIENTED_EDGE ( 'NONE', *, *, #19791, .T. ) ;
#14999 = EDGE_CURVE ( 'NONE', #1788, #3254, #4918, .T. ) ;
#15000 = EDGE_CURVE ( 'NONE', #5063, #15968, #1372, .T. ) ;
#15001 = CARTESIAN_POINT ( 'NONE',  ( 158.0000000000000568, 203.4448749474510407, 45.00000000000000000 ) ) ;
#15002 = CARTESIAN_POINT ( 'NONE',  ( -183.2595802227681361, 107.9574575171763655, -30.83290447571683046 ) ) ;
#15003 = ORIENTED_EDGE ( 'NONE', *, *, #14051, .F. ) ;
#15004 = VECTOR ( 'NONE', #14301, 1000.000000000000000 ) ;
#15005 = ORIENTED_EDGE ( 'NONE', *, *, #6319, .T. ) ;
#15006 = DIRECTION ( 'NONE',  ( 0.8916010070293437506, -0.4528218681383003874, 0.000000000000000000 ) ) ;
#15007 = ORIENTED_EDGE ( 'NONE', *, *, #9979, .F. ) ;
#15008 = EDGE_CURVE ( 'NONE', #5759, #3645, #7837, .T. ) ;
#15009 = VERTEX_POINT ( 'NONE', #27920 ) ;
#15010 = ORIENTED_EDGE ( 'NONE', *, *, #1754, .T. ) ;
#15011 = CARTESIAN_POINT ( 'NONE',  ( 9.345921402568901470, 140.0000000000000000, 15.00000000000000000 ) ) ;
#15012 = DIRECTION ( 'NONE',  ( 1.000000000000000000, 1.321694076934710155E-16, 0.000000000000000000 ) ) ;
#15013 = FACE_OUTER_BOUND ( 'NONE', #2783, .T. ) ;
#15014 = CARTESIAN_POINT ( 'NONE',  ( 232.4749999999995964, 83.06687458711267880, -36.86484227207694175 ) ) ;
#15015 = LINE ( 'NONE', #21183, #27098 ) ;
#15016 = DIRECTION ( 'NONE',  ( -0.000000000000000000, -0.000000000000000000, 1.000000000000000000 ) ) ;
#15017 = CARTESIAN_POINT ( 'NONE',  ( -230.6117145417363190, 64.61843588005640981, -16.59905221104221695 ) ) ;
#15018 = ORIENTED_EDGE ( 'NONE', *, *, #23113, .F. ) ;
#15019 = FACE_OUTER_BOUND ( 'NONE', #3595, .T. ) ;
#15020 = DIRECTION ( 'NONE',  ( 0.4767408570798813972, -0.8790438869537404720, 0.000000000000000000 ) ) ;
#15021 = CARTESIAN_POINT ( 'NONE',  ( 157.4999999999995453, 206.2066874587088989, 45.00000000000000000 ) ) ;
#15022 = FACE_OUTER_BOUND ( 'NONE', #5670, .T. ) ;
#15023 = CIRCLE ( 'NONE', #2615, 5.000000000000000888 ) ;
#15024 = VERTEX_POINT ( 'NONE', #9998 ) ;
#15025 = DIRECTION ( 'NONE',  ( 0.000000000000000000, 0.000000000000000000, 1.000000000000000000 ) ) ;
#15026 = TOROIDAL_SURFACE ( 'NONE', #17755, 60.59270260175150469, 2.000000000000000000 ) ;
#15027 = DIRECTION ( 'NONE',  ( 0.000000000000000000, 0.000000000000000000, -1.000000000000000000 ) ) ;
#15028 = CARTESIAN_POINT ( 'NONE',  ( -270.6285134702751520, -165.1572588087801421, 88.06168287673186512 ) ) ;
#15029 = LINE ( 'NONE', #1935, #24539 ) ;
#15030 = DIRECTION ( 'NONE',  ( 0.000000000000000000, -1.000000000000000000, 0.000000000000000000 ) ) ;
#15031 = ORIENTED_EDGE ( 'NONE', *, *, #20903, .T. ) ;
#15032 = CARTESIAN_POINT ( 'NONE',  ( 157.4999999999998579, 158.5570623160774630, -45.00000000000000000 ) ) ;
#15033 = ORIENTED_EDGE ( 'NONE', *, *, #6008, .T. ) ;
#15034 = LINE ( 'NONE', #24499, #21825 ) ;
#15035 = ORIENTED_EDGE ( 'NONE', *, *, #11875, .T. ) ;
#15036 = ORIENTED_EDGE ( 'NONE', *, *, #26998, .T. ) ;
#15037 = ADVANCED_FACE ( 'NONE', ( #15019 ), #27802, .T. ) ;
#15038 = DIRECTION ( 'NONE',  ( -1.321694076934710155E-16, 1.000000000000000000, 0.000000000000000000 ) ) ;
#15039 = VECTOR ( 'NONE', #27459, 1000.000000000000000 ) ;
#15040 = ORIENTED_EDGE ( 'NONE', *, *, #8614, .T. ) ;
#15041 = VERTEX_POINT ( 'NONE', #14456 ) ;
#15042 = DIRECTION ( 'NONE',  ( -0.000000000000000000, -0.000000000000000000, 1.000000000000000000 ) ) ;
#15043 = VECTOR ( 'NONE', #14341, 1000.000000000000000 ) ;
#15044 = PLANE ( 'NONE',  #26556 ) ;
#15045 = DIRECTION ( 'NONE',  ( -0.8916010070293409751, -0.4528218681383056610, 0.000000000000000000 ) ) ;
#15046 = CARTESIAN_POINT ( 'NONE',  ( -147.5692307249372277, 124.5789548200514218, -19.26288188869894924 ) ) ;
#15047 = B_SPLINE_CURVE_WITH_KNOTS ( 'NONE', 3,
 ( #3968, #1536, #28091, #12755, #10304, #21357, #8291, #17325, #17045, #2095, #25805, #23800, #19341, #19489, #19628, #24088, #21494, #1811, #8436, #23942, #6131, #19063, #17190, #10587, #25949, #10871, #27808, #16908 ),
 .UNSPECIFIED., .F., .F.,
 ( 4, 2, 2, 2, 2, 2, 2, 2, 2, 2, 2, 2, 2, 4 ),
 ( 0.000000000000000000, 0.007596912630457928854, 0.01139536894568684774, 0.01519382526091576577, 0.02279073789137358100, 0.03038765052183138929, 0.04558147578274701628, 0.06077530104366264674, 0.06457375735889157864, 0.06837221367412052442, 0.07596912630457833271, 0.09116295156549394929, 0.1063567768264095659, 0.1215506020873251825 ),
 .UNSPECIFIED. ) ;
#15048 = DIRECTION ( 'NONE',  ( 0.000000000000000000, 0.000000000000000000, 1.000000000000000000 ) ) ;
#15049 = CARTESIAN_POINT ( 'NONE',  ( 158.0000000000008527, 123.7007497147323960, 45.00000000000000000 ) ) ;
#15050 = CARTESIAN_POINT ( 'NONE',  ( -265.8373424361719799, -170.9544065693361290, 89.46035631147101697 ) ) ;
#15051 = CARTESIAN_POINT ( 'NONE',  ( -223.8731558706656699, 88.82041552423905273, -14.63364721595453233 ) ) ;
#15052 = DIRECTION ( 'NONE',  ( 0.000000000000000000, -1.000000000000000000, -1.214306433183764966E-16 ) ) ;
#15053 = DIRECTION ( 'NONE',  ( 0.8916010070296834789, -0.4528218681376312005, 0.000000000000000000 ) ) ;
#15054 = DIRECTION ( 'NONE',  ( 0.000000000000000000, -1.000000000000000000, 0.000000000000000000 ) ) ;
#15055 = PLANE ( 'NONE',  #21938 ) ;
#15056 = DIRECTION ( 'NONE',  ( 0.7071067811865613395, 0.7071067811865336949, 0.000000000000000000 ) ) ;
#15057 = ORIENTED_EDGE ( 'NONE', *, *, #11069, .F. ) ;
#15058 = AXIS2_PLACEMENT_3D ( 'NONE', #6455, #19953, #6600 ) ;
#15059 = EDGE_CURVE ( 'NONE', #8019, #26636, #5339, .T. ) ;
#15060 = AXIS2_PLACEMENT_3D ( 'NONE', #21295, #7806, #3764 ) ;
#15061 = CARTESIAN_POINT ( 'NONE',  ( -40.40953891503691153, 0.000000000000000000, 99.00000000000000000 ) ) ;
#15062 = FACE_OUTER_BOUND ( 'NONE', #16136, .T. ) ;
#15063 = DIRECTION ( 'NONE',  ( 0.000000000000000000, 0.000000000000000000, 1.000000000000000000 ) ) ;
#15064 =( BOUNDED_SURFACE ( )  B_SPLINE_SURFACE ( 3, 2, ( 
 ( #9206, #26426, #24284 ),
 ( #20257, #26571, #15679 ),
 ( #7047, #11367, #303 ),
 ( #15967, #15536, #24858 ),
 ( #13814, #24428, #2728 ),
 ( #11075, #13523, #728 ),
 ( #22564, #24716, #17966 ),
 ( #9498, #20400, #11222 ),
 ( #9059, #8919, #11664 ),
 ( #18253, #27005, #9353 ),
 ( #22274, #7194, #26717 ),
 ( #15829, #22128, #16108 ),
 ( #5172, #24572, #18112 ),
 ( #4883, #2872, #19829 ),
 ( #157, #17673, #4592 ),
 ( #13378, #12328, #19058 ),
 ( #8140, #5704, #5979 ),
 ( #18392, #12467, #17040 ),
 ( #6127, #23365, #8002 ),
 ( #27145, #21068, #10299 ),
 ( #6263, #7479, #16249 ),
 ( #24997, #28084, #3678 ),
 ( #25800, #1391, #14476 ),
 ( #23654, #3964, #23233 ),
 ( #20540, #3535, #16769 ),
 ( #10160, #3009, #14902 ),
 ( #21207, #14611, #25521 ),
 ( #25654, #12750, #18914 ) ),
 .UNSPECIFIED., .F., .F., .T. ) 
 B_SPLINE_SURFACE_WITH_KNOTS ( ( 4, 2, 2, 2, 2, 2, 2, 2, 2, 2, 2, 2, 2, 4 ),
 ( 3, 3 ),
 ( 0.000000000000000000, 0.007529199611455438673, 0.01505839922291087735, 0.02258759883436631602, 0.02635219864009403362, 0.03011679844582175469, 0.04517519766873263204, 0.06023359689164350939, 0.07529199611455439367, 0.07905659592028210780, 0.08282119572600982194, 0.09035039533746526408, 0.1054087945603761345, 0.1204671937832870188 ),
 ( 0.000000000000000000, 1.000000000000000000 ),
 .UNSPECIFIED. ) 
 GEOMETRIC_REPRESENTATION_ITEM ( )  RATIONAL_B_SPLINE_SURFACE ( (
 ( 1.000000000000000000, 0.8981184559478656571, 1.000000000000000000),
 ( 1.000000000000000000, 0.8913409640699760939, 1.000000000000000000),
 ( 1.000000000000000000, 0.8845625463580112369, 1.000000000000000000),
 ( 1.000000000000000000, 0.8711578316887859108, 1.000000000000000000),
 ( 1.000000000000000000, 0.8645314129694308125, 1.000000000000000000),
 ( 1.000000000000000000, 0.8515750003171709270, 1.000000000000000000),
 ( 1.000000000000000000, 0.8452448728250648857, 1.000000000000000000),
 ( 1.000000000000000000, 0.8360775906454407380, 1.000000000000000000),
 ( 1.000000000000000000, 0.8330764670878353373, 1.000000000000000000),
 ( 1.000000000000000000, 0.8272009908158640679, 1.000000000000000000),
 ( 1.000000000000000000, 0.8243270960686099880, 1.000000000000000000),
 ( 1.000000000000000000, 0.8103905206081341017, 1.000000000000000000),
 ( 1.000000000000000000, 0.8005641981319898681, 1.000000000000000000),
 ( 1.000000000000000000, 0.7842823063492941893, 1.000000000000000000),
 ( 1.000000000000000000, 0.7778294879052323196, 1.000000000000000000),
 ( 1.000000000000000000, 0.7688627540743353528, 1.000000000000000000),
 ( 1.000000000000000000, 0.7663513471414680200, 1.000000000000000000),
 ( 1.000000000000000000, 0.7658761447369581976, 1.000000000000000000),
 ( 1.000000000000000000, 0.7659136159393603593, 1.000000000000000000),
 ( 1.000000000000000000, 0.7662557092201324194, 1.000000000000000000),
 ( 1.000000000000000000, 0.7665607478393150487, 1.000000000000000000),
 ( 1.000000000000000000, 0.7678709653268237512, 1.000000000000000000),
 ( 1.000000000000000000, 0.7692719988712057866, 1.000000000000000000),
 ( 1.000000000000000000, 0.7749914125728452063, 1.000000000000000000),
 ( 1.000000000000000000, 0.7808328044829244696, 1.000000000000000000),
 ( 1.000000000000000000, 0.7960310293872467913, 1.000000000000000000),
 ( 1.000000000000000000, 0.8053828549108267287, 1.000000000000000000),
 ( 1.000000000000000000, 0.8161343730438193056, 1.000000000000000000) ) ) 
 REPRESENTATION_ITEM ( '' )  SURFACE ( )  );
#15065 = ORIENTED_EDGE ( 'NONE', *, *, #24211, .T. ) ;
#15066 = CARTESIAN_POINT ( 'NONE',  ( 104.4928295061288281, 246.1605864358141673, -20.56267333362882255 ) ) ;
#15067 = ORIENTED_EDGE ( 'NONE', *, *, #3016, .T. ) ;
#15068 = CARTESIAN_POINT ( 'NONE',  ( -273.6211430000234373, -91.18033988749901653, 0.000000000000000000 ) ) ;
#15069 = ORIENTED_EDGE ( 'NONE', *, *, #12097, .F. ) ;
#15070 = EDGE_CURVE ( 'NONE', #9313, #21412, #1230, .T. ) ;
#15071 = ORIENTED_EDGE ( 'NONE', *, *, #18828, .F. ) ;
#15072 = EDGE_CURVE ( 'NONE', #9774, #14497, #19317, .T. ) ;
#15073 = ADVANCED_FACE ( 'NONE', ( #28062 ), #25776, .F. ) ;
#15074 = VECTOR ( 'NONE', #9866, 1000.000000000000000 ) ;
#15075 = EDGE_CURVE ( 'NONE', #3625, #5724, #10142, .T. ) ;
#15076 = VERTEX_POINT ( 'NONE', #352 ) ;
#15077 = VERTEX_POINT ( 'NONE', #4497 ) ;
#15078 = VERTEX_POINT ( 'NONE', #17870 ) ;
#15079 = DIRECTION ( 'NONE',  ( -1.224646799147353207E-16, 1.000000000000000000, 0.000000000000000000 ) ) ;
#15080 = VECTOR ( 'NONE', #19640, 1000.000000000000000 ) ;
#15081 = AXIS2_PLACEMENT_3D ( 'NONE', #3264, #1121, #18786 ) ;
#15082 = CARTESIAN_POINT ( 'NONE',  ( 93.17300876009500143, -24.96563245364655259, -45.00000000000000000 ) ) ;
#15083 = CARTESIAN_POINT ( 'NONE',  ( -58.76345596729049703, 58.76345596729049703, 45.00000000000000000 ) ) ;
#15084 = CARTESIAN_POINT ( 'NONE',  ( 65.00000000000000000, -150.0000000000000568, -64.00000000000000000 ) ) ;
#15085 = CARTESIAN_POINT ( 'NONE',  ( -175.0000000000000000, -120.0000000000001847, -69.99999999999998579 ) ) ;
#15086 = CARTESIAN_POINT ( 'NONE',  ( 127.3463313526980727, 238.4775906502252667, -45.00000000000000000 ) ) ;
#15087 = CARTESIAN_POINT ( 'NONE',  ( -236.8177751472017007, 82.33896643611701904, -15.00000000000000000 ) ) ;
#15089 = VECTOR ( 'NONE', #10210, 1000.000000000000000 ) ;
#15088 = CARTESIAN_POINT ( 'NONE',  ( -24.75943805428697786, 129.2472029784736662, 15.64972235346578167 ) ) ;
#15090 = PLANE ( 'NONE',  #3161 ) ;
#15091 = DIRECTION ( 'NONE',  ( 0.000000000000000000, 0.000000000000000000, 1.000000000000000000 ) ) ;
#15092 = CARTESIAN_POINT ( 'NONE',  ( 157.4999999999998579, 178.6200623761337738, -45.00000000000000000 ) ) ;
#15093 = VERTEX_POINT ( 'NONE', #15308 ) ;
#15094 = CARTESIAN_POINT ( 'NONE',  ( 179.9999999999999147, -5.589247009368157215, 84.99999999999997158 ) ) ;
#15095 = ADVANCED_FACE ( 'NONE', ( #6669 ), #15448, .T. ) ;
#15096 = AXIS2_PLACEMENT_3D ( 'NONE', #6672, #20459, #2637 ) ;
#15097 = ADVANCED_FACE ( 'NONE', ( #8967 ), #28341, .F. ) ;
#15098 = PRODUCT_DEFINITION_SHAPE ( 'NONE', 'NONE',  #28412 ) ;
#15099 = VECTOR ( 'NONE', #12092, 1000.000000000000227 ) ;
#15100 = CARTESIAN_POINT ( 'NONE',  ( -277.5909579262273041, -164.9999999998546798, -106.8329485552555269 ) ) ;
#15101 = ORIENTED_EDGE ( 'NONE', *, *, #8298, .T. ) ;
#15102 = ITEM_DEFINED_TRANSFORMATION ( 'NONE', 'NONE', #9273,  #10637 ) ;
#15103 = VERTEX_POINT ( 'NONE', #24196 ) ;
#15105 = VERTEX_POINT ( 'NONE', #22182 ) ;
#15104 = AXIS2_PLACEMENT_3D ( 'NONE', #20859, #11974, #18843 ) ;
#15106 = DIRECTION ( 'NONE',  ( 0.000000000000000000, -1.000000000000000000, -1.214306433183764966E-16 ) ) ;
#15107 = CARTESIAN_POINT ( 'NONE',  ( 157.9999999999998579, 0.000000000000000000, 45.00000000000000000 ) ) ;
#15108 = ADVANCED_FACE ( 'NONE', ( #1924 ), #2486, .F. ) ;
#15109 = ORIENTED_EDGE ( 'NONE', *, *, #12775, .T. ) ;
#15110 = ORIENTED_EDGE ( 'NONE', *, *, #20387, .F. ) ;
#15111 = CARTESIAN_POINT ( 'NONE',  ( 109.5756401947800356, 134.3783162856662159, -100.0000000000000142 ) ) ;
#15112 = EDGE_CURVE ( 'NONE', #24882, #15116, #6526, .T. ) ;
#15113 = CARTESIAN_POINT ( 'NONE',  ( 92.44907173541768941, 230.7276239336879371, 17.70004142540128456 ) ) ;
#15114 = DIRECTION ( 'NONE',  ( 1.000000000000000000, 0.000000000000000000, 0.000000000000000000 ) ) ;
#15115 = COLOUR_RGB ( '',0.7921568627450980005, 0.8196078431372548767, 0.9333333333333333481 ) ;
#15116 = VERTEX_POINT ( 'NONE', #13155 ) ;
#15117 = CARTESIAN_POINT ( 'NONE',  ( -216.2392880859841284, 87.80609967497970558, 20.45738389094162457 ) ) ;
#15118 = VERTEX_POINT ( 'NONE', #28204 ) ;
#15119 = CARTESIAN_POINT ( 'NONE',  ( 157.4999999999998579, 80.81293708335913095, -45.00000000000000000 ) ) ;
#15120 = VECTOR ( 'NONE', #14356, 1000.000000000000000 ) ;
#15121 = CARTESIAN_POINT ( 'NONE',  ( 90.00000000000042633, 230.0000000000000284, -6.270166537925968342 ) ) ;
#15122 = PLANE ( 'NONE',  #23290 ) ;
#15123 = VECTOR ( 'NONE', #27011, 1000.000000000000000 ) ;
#15124 = PLANE ( 'NONE',  #23442 ) ;
#15125 = EDGE_LOOP ( 'NONE', ( #27208, #25576, #1665, #12008 ) ) ;
#15126 = FACE_BOUND ( 'NONE', #22377, .T. ) ;
#15127 = CARTESIAN_POINT ( 'NONE',  ( -21.33210486176665910, 0.000000000000000000, 99.00000000000000000 ) ) ;
#15128 = FACE_OUTER_BOUND ( 'NONE', #8792, .T. ) ;
#15129 = DIRECTION ( 'NONE',  ( 0.000000000000000000, -1.000000000000000000, -1.214306433183764966E-16 ) ) ;
#15130 = ORIENTED_EDGE ( 'NONE', *, *, #8022, .F. ) ;
#15131 = DIRECTION ( 'NONE',  ( -0.000000000000000000, -0.000000000000000000, -1.000000000000000000 ) ) ;
#15132 = EDGE_CURVE ( 'NONE', #24416, #2973, #11125, .T. ) ;
#15133 = CARTESIAN_POINT ( 'NONE',  ( 157.9999999999998295, 231.0315000300280417, 45.00000000000000000 ) ) ;
#15134 = DIRECTION ( 'NONE',  ( -0.000000000000000000, -0.000000000000000000, -1.000000000000000000 ) ) ;
#15135 = CARTESIAN_POINT ( 'NONE',  ( -226.7417855643314226, 89.97934261517927723, 13.71636754133556302 ) ) ;
#15136 = ORIENTED_EDGE ( 'NONE', *, *, #7453, .T. ) ;
#15137 = SHAPE_REPRESENTATION_RELATIONSHIP ( 'NONE' , 'NONE' ,  #26803, #7469 ) ;
#15138 = CARTESIAN_POINT ( 'NONE',  ( -63.57415822541634043, 80.97823757117562593, 95.00000000000000000 ) ) ;
#15139 = ORIENTED_EDGE ( 'NONE', *, *, #6623, .T. ) ;
#15140 = VECTOR ( 'NONE', #18488, 1000.000000000000227 ) ;
#15141 = DIRECTION ( 'NONE',  ( -0.9659258262890662028, 0.2588190451025286221, 0.000000000000000000 ) ) ;
#15142 = CARTESIAN_POINT ( 'NONE',  ( -187.2788549371262832, 105.2860637900685674, -32.19960561888341743 ) ) ;
#15143 = VERTEX_POINT ( 'NONE', #22038 ) ;
#15144 = ORIENTED_EDGE ( 'NONE', *, *, #495, .F. ) ;
#15145 = CARTESIAN_POINT ( 'NONE',  ( -68.57415822541635464, 75.97823757117562593, 80.00000000000001421 ) ) ;
#15146 = VERTEX_POINT ( 'NONE', #19882 ) ;
#15147 = EDGE_CURVE ( 'NONE', #19302, #18838, #208, .T. ) ;
#15148 = LINE ( 'NONE', #19724, #1988 ) ;
#15149 = EDGE_CURVE ( 'NONE', #8625, #1736, #2068, .T. ) ;
#15150 = EDGE_LOOP ( 'NONE', ( #27240, #4956, #1355, #15394 ) ) ;
#15151 = ORIENTED_EDGE ( 'NONE', *, *, #26628, .F. ) ;
#15152 = CARTESIAN_POINT ( 'NONE',  ( 157.4999999999994600, 213.7303124812313513, -45.00000000000000000 ) ) ;
#15153 = VECTOR ( 'NONE', #22650, 1000.000000000000000 ) ;
#15154 = B_SPLINE_CURVE_WITH_KNOTS ( 'NONE', 3,
 ( #11757, #14053, #22802, #20497, #25643, #16890, #3812 ),
 .UNSPECIFIED., .F., .F.,
 ( 4, 3, 4 ),
 ( 0.01306422253233230878, 0.01395283648363494430, 0.01510707358649056309 ),
 .UNSPECIFIED. ) ;
#15155 = DIRECTION ( 'NONE',  ( 0.9960550913260672878, 0.000000000000000000, -0.08873699929240054518 ) ) ;
#15156 = CARTESIAN_POINT ( 'NONE',  ( 0.1707425712781837635, 1.249999999999999556, 7.345313475977262030 ) ) ;
#15157 = DIRECTION ( 'NONE',  ( -0.8916010070295719014, 0.4528218681378510801, 0.000000000000000000 ) ) ;
#15158 = B_SPLINE_CURVE_WITH_KNOTS ( 'NONE', 3,
 ( #15565, #16692, #25443, #7784, #14400, #23153, #16415 ),
 .UNSPECIFIED., .F., .F.,
 ( 4, 3, 4 ),
 ( 0.01279859917594709795, 0.01395283628746607149, 0.01484145024773051748 ),
 .UNSPECIFIED. ) ;
#15159 = ADVANCED_FACE ( 'NONE', ( #9110 ), #26340, .F. ) ;
#15160 = DIRECTION ( 'NONE',  ( 0.000000000000000000, 0.000000000000000000, 1.000000000000000000 ) ) ;
#15161 = VECTOR ( 'NONE', #14021, 1000.000000000000000 ) ;
#15162 = LINE ( 'NONE', #13153, #3615 ) ;
#15163 = CARTESIAN_POINT ( 'NONE',  ( -237.6054256748464013, 69.18099216265484586, -14.87827728787998538 ) ) ;
#15164 = ORIENTED_EDGE ( 'NONE', *, *, #9758, .F. ) ;
#15165 = EDGE_CURVE ( 'NONE', #8650, #14563, #19738, .T. ) ;
#15166 = CARTESIAN_POINT ( 'NONE',  ( 113.4538925329242574, 207.5603490538955782, -151.0000000000000284 ) ) ;
#15167 = DIRECTION ( 'NONE',  ( -0.8916010070293383105, -0.4528218681383106015, 0.000000000000000000 ) ) ;
#15168 = CARTESIAN_POINT ( 'NONE',  ( 157.9999999999999432, 211.4763749774776045, -45.00000000000000000 ) ) ;
#15169 = CARTESIAN_POINT ( 'NONE',  ( 112.5248869502488986, 215.0130877889307044, 45.00000000000000000 ) ) ;
#15170 = ORIENTED_EDGE ( 'NONE', *, *, #17813, .F. ) ;
#15171 = CARTESIAN_POINT ( 'NONE',  ( 158.0000000000002558, 183.3818748873943889, 45.00000000000000000 ) ) ;
#15172 = CARTESIAN_POINT ( 'NONE',  ( 134.9999999999998579, 220.0000000000000284, -119.9999999999999858 ) ) ;
#15173 = PLANE ( 'NONE',  #3656 ) ;
#15174 = FACE_OUTER_BOUND ( 'NONE', #3049, .T. ) ;
#15175 = DIRECTION ( 'NONE',  ( 1.000000000000000000, 0.000000000000000000, 0.000000000000000000 ) ) ;
#15176 = EDGE_LOOP ( 'NONE', ( #17732, #20157, #3171, #12647 ) ) ;
#15177 = TOROIDAL_SURFACE ( 'NONE', #6898, 421.5408555545579929, 7.500000000000000000 ) ;
#15178 = CARTESIAN_POINT ( 'NONE',  ( 150.8670668058245212, 232.1752285801742630, 45.00000000000000000 ) ) ;
#15179 = EDGE_LOOP ( 'NONE', ( #22272, #19906, #7555, #26531 ) ) ;
#15180 = CARTESIAN_POINT ( 'NONE',  ( -266.5073747506846189, -165.8832655043242994, 109.6017926887263343 ) ) ;
#15181 = ORIENTED_EDGE ( 'NONE', *, *, #27696, .F. ) ;
#15182 = EDGE_LOOP ( 'NONE', ( #4928, #11094, #3449, #13092 ) ) ;
#15183 = EDGE_CURVE ( 'NONE', #5204, #16487, #4488, .T. ) ;
#15184 = DIRECTION ( 'NONE',  ( 0.000000000000000000, 0.000000000000000000, 1.000000000000000000 ) ) ;
#15185 = VECTOR ( 'NONE', #1474, 1000.000000000000114 ) ;
#15186 = EDGE_CURVE ( 'NONE', #3239, #14756, #27886, .T. ) ;
#15187 = VERTEX_POINT ( 'NONE', #8824 ) ;
#15188 = VERTEX_POINT ( 'NONE', #17583 ) ;
#15189 = CARTESIAN_POINT ( 'NONE',  ( -227.8378063125350650, 130.6400894613934724, 15.00000000000001954 ) ) ;
#15190 = CARTESIAN_POINT ( 'NONE',  ( 134.9999999999998579, 220.0000000000000284, 84.99999999999995737 ) ) ;
#15191 = CARTESIAN_POINT ( 'NONE',  ( -212.8298628423295895, -217.6190342207067943, 94.05759435423763648 ) ) ;
#15192 = LINE ( 'NONE', #2375, #26847 ) ;
#15193 = CARTESIAN_POINT ( 'NONE',  ( 158.0000000000016485, 50.46449948952111697, -45.00000000000000000 ) ) ;
#15194 = CARTESIAN_POINT ( 'NONE',  ( 139.9999999999999432, -90.00000000000000000, -70.00000000000001421 ) ) ;
#15195 = CARTESIAN_POINT ( 'NONE',  ( -273.6825128178298883, -170.0454220111860764, 86.72654589157289706 ) ) ;
#15196 = CARTESIAN_POINT ( 'NONE',  ( -214.1881881672503312, 87.99490168924762656, -20.10759990481813375 ) ) ;
#15197 = VECTOR ( 'NONE', #10807, 1000.000000000000000 ) ;
#15198 = CARTESIAN_POINT ( 'NONE',  ( -175.0000000000000000, -170.0000000000001990, -75.99999999999995737 ) ) ;
#15199 = DIRECTION ( 'NONE',  ( -0.8916010070295314893, -0.4528218681379303501, 0.000000000000000000 ) ) ;
#15200 = FACE_OUTER_BOUND ( 'NONE', #16768, .T. ) ;
#15201 = DIRECTION ( 'NONE',  ( 1.000000000000000000, 0.000000000000000000, 0.000000000000000000 ) ) ;
#15202 = CARTESIAN_POINT ( 'NONE',  ( 158.0000000000009379, 118.1771246922112653, -45.00000000000000000 ) ) ;
#15203 = EDGE_CURVE ( 'NONE', #2227, #26033, #19192, .T. ) ;
#15204 = ORIENTED_EDGE ( 'NONE', *, *, #19633, .F. ) ;
#15205 = FACE_OUTER_BOUND ( 'NONE', #2825, .T. ) ;
#15206 = EDGE_CURVE ( 'NONE', #8537, #12718, #15583, .T. ) ;
#15207 = AXIS2_PLACEMENT_3D ( 'NONE', #7772, #16677, #13977 ) ;
#15208 = CARTESIAN_POINT ( 'NONE',  ( 109.9999999999999005, 140.0000000000000284, 91.30899693899577585 ) ) ;
#15209 = DIRECTION ( 'NONE',  ( 0.000000000000000000, -1.000000000000000000, 0.000000000000000000 ) ) ;
#15210 = EDGE_CURVE ( 'NONE', #7037, #11558, #12869, .T. ) ;
#15211 = CARTESIAN_POINT ( 'NONE',  ( 106.5943545129268273, 210.3500852710297124, -146.3660979730027520 ) ) ;
#15212 = ORIENTED_EDGE ( 'NONE', *, *, #4624, .F. ) ;
#15213 = CARTESIAN_POINT ( 'NONE',  ( 98.38958437017922165, 241.8303606468361409, -11.96405203492589564 ) ) ;
#15214 = ORIENTED_EDGE ( 'NONE', *, *, #26653, .F. ) ;
#15215 = CARTESIAN_POINT ( 'NONE',  ( 0.6789813131199424756, 136.5995534334086301, -13.39369412120168157 ) ) ;
#15216 = ORIENTED_EDGE ( 'NONE', *, *, #17205, .T. ) ;
#15217 = ORIENTED_EDGE ( 'NONE', *, *, #25952, .T. ) ;
#15218 = VECTOR ( 'NONE', #12628, 1000.000000000000000 ) ;
#15219 = VERTEX_POINT ( 'NONE', #20593 ) ;
#15220 = EDGE_LOOP ( 'NONE', ( #4353, #10002, #22478, #23259 ) ) ;
#15221 = ORIENTED_EDGE ( 'NONE', *, *, #9683, .F. ) ;
#15222 =( GEOMETRIC_REPRESENTATION_CONTEXT ( 3 ) GLOBAL_UNCERTAINTY_ASSIGNED_CONTEXT ( ( #19802 ) ) GLOBAL_UNIT_ASSIGNED_CONTEXT ( ( #6958, #22483, #11581 ) ) REPRESENTATION_CONTEXT ( 'NONE', 'WORKASPACE' ) );
#15223 = FACE_OUTER_BOUND ( 'NONE', #23997, .T. ) ;
#15224 = VECTOR ( 'NONE', #9454, 1000.000000000000000 ) ;
#15225 = CARTESIAN_POINT ( 'NONE',  ( 65.00000000000000000, -120.0000000000000711, 70.00000000000001421 ) ) ;
#15226 = CARTESIAN_POINT ( 'NONE',  ( 158.0000000000003695, 173.3503748573662051, 45.00000000000000000 ) ) ;
#15227 = DIRECTION ( 'NONE',  ( -0.000000000000000000, -0.000000000000000000, -1.000000000000000000 ) ) ;
#15228 = DIRECTION ( 'NONE',  ( -0.5457381880580680633, 0.8379557447115549840, 0.000000000000000000 ) ) ;
#15229 = FACE_OUTER_BOUND ( 'NONE', #997, .T. ) ;
#15230 = CARTESIAN_POINT ( 'NONE',  ( 158.0000000000013358, 80.55899957960563995, 45.00000000000000000 ) ) ;
#15231 = ADVANCED_FACE ( 'NONE', ( #917 ), #5224, .F. ) ;
#15232 = CARTESIAN_POINT ( 'NONE',  ( -210.0000000000000568, -210.8114316696540982, -89.99999999999987210 ) ) ;
#15233 = DIRECTION ( 'NONE',  ( 1.000000000000000000, 0.000000000000000000, 0.000000000000000000 ) ) ;
#15234 = EDGE_CURVE ( 'NONE', #7395, #11330, #7099, .T. ) ;
#15235 = VECTOR ( 'NONE', #25599, 1000.000000000000000 ) ;
#15236 = CARTESIAN_POINT ( 'NONE',  ( 157.9999999999998010, 234.0472500450420341, 45.00000000000000000 ) ) ;
#15237 = ADVANCED_FACE ( 'NONE', ( #15879 ), #14143, .F. ) ;
#15238 = CARTESIAN_POINT ( 'NONE',  ( 134.9999999999998579, 404.6636166603179277, -145.0000000000000000 ) ) ;
#15239 = CARTESIAN_POINT ( 'NONE',  ( 157.4999999999997726, 248.8405625863305204, 45.00000000000000000 ) ) ;
#15240 = DIRECTION ( 'NONE',  ( -1.000000000000000000, -0.000000000000000000, -0.000000000000000000 ) ) ;
#15241 = VECTOR ( 'NONE', #10123, 1000.000000000000000 ) ;
#15243 = ORIENTED_EDGE ( 'NONE', *, *, #7192, .T. ) ;
#15242 = VERTEX_POINT ( 'NONE', #9685 ) ;
#15244 =( GEOMETRIC_REPRESENTATION_CONTEXT ( 3 ) GLOBAL_UNCERTAINTY_ASSIGNED_CONTEXT ( ( #18368 ) ) GLOBAL_UNIT_ASSIGNED_CONTEXT ( ( #8943, #4618, #6779 ) ) REPRESENTATION_CONTEXT ( 'NONE', 'WORKASPACE' ) );
#15245 = CARTESIAN_POINT ( 'NONE',  ( -178.8123904115888934, 110.7331632632894411, 29.85040004129419700 ) ) ;
#15246 = AXIS2_PLACEMENT_3D ( 'NONE', #24922, #5517, #5091 ) ;
#15247 = DIRECTION ( 'NONE',  ( 0.000000000000000000, -1.000000000000000000, 0.000000000000000000 ) ) ;
#15248 = ORIENTED_EDGE ( 'NONE', *, *, #25482, .F. ) ;
#15249 = APPLICATION_PROTOCOL_DEFINITION ( 'draft international standard', 'automotive_design', 1998, #24702 ) ;
#15250 = ORIENTED_EDGE ( 'NONE', *, *, #3358, .T. ) ;
#15251 = ORIENTED_EDGE ( 'NONE', *, *, #22635, .T. ) ;
#15252 = CARTESIAN_POINT ( 'NONE',  ( -160.8326600028555902, 120.2355194873575073, -21.37420696376537776 ) ) ;
#15253 = DIRECTION ( 'NONE',  ( -0.000000000000000000, 1.000000000000000000, -1.387778780781445429E-16 ) ) ;
#15254 = ORIENTED_EDGE ( 'NONE', *, *, #6654, .T. ) ;
#15255 = VECTOR ( 'NONE', #12198, 1000.000000000000000 ) ;
#15256 = CARTESIAN_POINT ( 'NONE',  ( 105.2480867104912790, 123.6573351778161793, -99.99999999997838529 ) ) ;
#15257 = VECTOR ( 'NONE', #6918, 1000.000000000000000 ) ;
#15258 = CARTESIAN_POINT ( 'NONE',  ( 157.4999999999998579, 128.4625622259929401, 45.00000000000000000 ) ) ;
#15259 = EDGE_LOOP ( 'NONE', ( #4524, #7689 ) ) ;
#15260 = CARTESIAN_POINT ( 'NONE',  ( -229.0920485471770860, 88.91763133824811405, 15.43435999875618236 ) ) ;
#15261 = ORIENTED_EDGE ( 'NONE', *, *, #13932, .F. ) ;
#15262 = AXIS2_PLACEMENT_3D ( 'NONE', #9148, #24366, #15483 ) ;
#15263 = CARTESIAN_POINT ( 'NONE',  ( 157.9999999999998295, 231.0315000300280417, 45.00000000000000000 ) ) ;
#15264 = AXIS2_PLACEMENT_3D ( 'NONE', #3918, #7819, #21444 ) ;
#15265 = EDGE_CURVE ( 'NONE', #1736, #6015, #9255, .T. ) ;
#15266 = CARTESIAN_POINT ( 'NONE',  ( 367.4999999999996021, -5.589247009368160768, 100.0000000000000284 ) ) ;
#15267 = CARTESIAN_POINT ( 'NONE',  ( 160.1689500485674955, 203.6733438637415645, -150.7983993365949971 ) ) ;
#15268 = ADVANCED_FACE ( 'NONE', ( #18444 ), #13867, .F. ) ;
#15269 = DIRECTION ( 'NONE',  ( -0.000000000000000000, 0.000000000000000000, -1.000000000000000000 ) ) ;
#15270 = ORIENTED_EDGE ( 'NONE', *, *, #4183, .F. ) ;
#15271 = CARTESIAN_POINT ( 'NONE',  ( 65.00000000000000000, -170.0000000000000568, 76.00000000000000000 ) ) ;
#15272 = ADVANCED_FACE ( 'NONE', ( #20730, #11711, #18020, #22760, #20456 ), #780, .F. ) ;
#15273 = VECTOR ( 'NONE', #5148, 1000.000000000000114 ) ;
#15274 = FACE_OUTER_BOUND ( 'NONE', #7301, .T. ) ;
#15275 = LINE ( 'NONE', #21727, #8355 ) ;
#15276 = DIRECTION ( 'NONE',  ( 1.000000000000000000, 0.000000000000000000, -0.000000000000000000 ) ) ;
#15277 = VERTEX_POINT ( 'NONE', #1056 ) ;
#15278 = VECTOR ( 'NONE', #24686, 1000.000000000000000 ) ;
#15279 = FACE_OUTER_BOUND ( 'NONE', #23160, .T. ) ;
#15280 = VECTOR ( 'NONE', #17374, 1000.000000000000000 ) ;
#15281 = CARTESIAN_POINT ( 'NONE',  ( 157.4999999999998579, 43.19481197075347723, 45.00000000000000000 ) ) ;
#15282 = CARTESIAN_POINT ( 'NONE',  ( 184.9999999999999147, -150.0000000000000284, 84.99999999999995737 ) ) ;
#15283 = ORIENTED_EDGE ( 'NONE', *, *, #17292, .T. ) ;
#15284 =( LENGTH_UNIT ( ) NAMED_UNIT ( * ) SI_UNIT ( .MILLI., .METRE. ) );
#15285 = CIRCLE ( 'NONE', #18941, 2.000000000000000444 ) ;
#15286 = ORIENTED_EDGE ( 'NONE', *, *, #12141, .T. ) ;
#15287 = VECTOR ( 'NONE', #1211, 1000.000000000000000 ) ;
#15288 = DIRECTION ( 'NONE',  ( 1.000000000000000000, 0.000000000000000000, 0.000000000000000000 ) ) ;
#15289 = CARTESIAN_POINT ( 'NONE',  ( -189.4726776444009317, 103.5548156087989184, -32.83427761469911843 ) ) ;
#15290 = ORIENTED_EDGE ( 'NONE', *, *, #26347, .F. ) ;
#15291 = EDGE_LOOP ( 'NONE', ( #19788, #16996, #26634, #21292 ) ) ;
#15292 = CARTESIAN_POINT ( 'NONE',  ( -114.3540299464916785, 71.47411450562970003, 82.81256190651343729 ) ) ;
#15293 = LINE ( 'NONE', #24048, #5213 ) ;
#15295 = ADVANCED_FACE ( 'NONE', ( #3201 ), #14009, .F. ) ;
#15294 = ORIENTED_EDGE ( 'NONE', *, *, #12296, .F. ) ;
#15296 = ORIENTED_EDGE ( 'NONE', *, *, #7986, .T. ) ;
#15297 = CARTESIAN_POINT ( 'NONE',  ( 156.5461074670752453, 207.5603490538953224, -138.9999999999999432 ) ) ;
#15298 = EDGE_CURVE ( 'NONE', #7085, #23833, #22471, .T. ) ;
#15299 = CIRCLE ( 'NONE', #8423, 55.86582179324592090 ) ;
#15300 = DIRECTION ( 'NONE',  ( 1.000000000000000000, 0.000000000000000000, 0.000000000000000000 ) ) ;
#15301 = DIRECTION ( 'NONE',  ( 0.000000000000000000, -1.000000000000000000, 0.000000000000000000 ) ) ;
#15302 = DIRECTION ( 'NONE',  ( 1.000000000000000000, 0.000000000000000000, 0.000000000000000000 ) ) ;
#15303 = CIRCLE ( 'NONE', #9332, 562.1290781602207289 ) ;
#15304 = DIRECTION ( 'NONE',  ( 0.8379557447115657531, 0.5457381880580516320, 0.000000000000000000 ) ) ;
#15305 = CARTESIAN_POINT ( 'NONE',  ( 158.0000000000005400, 156.3031248123239436, 45.00000000000000000 ) ) ;
#15306 = FACE_OUTER_BOUND ( 'NONE', #15179, .T. ) ;
#15307 = ORIENTED_EDGE ( 'NONE', *, *, #15000, .T. ) ;
#15308 = CARTESIAN_POINT ( 'NONE',  ( 124.9999999999998579, 220.0000000000000284, 109.9999999999999858 ) ) ;
#15309 = EDGE_CURVE ( 'NONE', #11692, #21431, #24626, .T. ) ;
#15310 = DIRECTION ( 'NONE',  ( 0.4528218681382463751, 0.8916010070293711731, -0.000000000000000000 ) ) ;
#15311 = CARTESIAN_POINT ( 'NONE',  ( 367.4999999999996021, -5.589247009368149222, 1.243177022048955014E-14 ) ) ;
#15312 = DIRECTION ( 'NONE',  ( -0.8916010070293409751, -0.4528218681383056610, 0.000000000000000000 ) ) ;
#15313 = ORIENTED_EDGE ( 'NONE', *, *, #12617, .T. ) ;
#15314 = FACE_OUTER_BOUND ( 'NONE', #20288, .T. ) ;
#15315 = EDGE_CURVE ( 'NONE', #8063, #19692, #11989, .T. ) ;
#15316 = DIRECTION ( 'NONE',  ( 0.000000000000000000, 0.000000000000000000, 1.000000000000000000 ) ) ;
#15317 = CARTESIAN_POINT ( 'NONE',  ( -268.7788207492064316, -165.3337907801079325, 88.69420594919965595 ) ) ;
#15318 = DIRECTION ( 'NONE',  ( 1.000000000000000000, 0.000000000000000000, 2.064684994405763843E-16 ) ) ;
#15319 = CARTESIAN_POINT ( 'NONE',  ( 157.9999999999998579, 221.0000000000000284, 45.00000000000000000 ) ) ;
#15320 = CARTESIAN_POINT ( 'NONE',  ( 157.4999999999996874, 268.9035626463865469, -45.00000000000000000 ) ) ;
#15321 = VERTEX_POINT ( 'NONE', #27329 ) ;
#15322 = VECTOR ( 'NONE', #11673, 1000.000000000000000 ) ;
#15323 = AXIS2_PLACEMENT_3D ( 'NONE', #24317, #339, #4774 ) ;
#15324 = CARTESIAN_POINT ( 'NONE',  ( -220.8227294558590756, 71.35641261643398536, 21.08939097871950707 ) ) ;
#15325 = ORIENTED_EDGE ( 'NONE', *, *, #15688, .T. ) ;
#15326 = CARTESIAN_POINT ( 'NONE',  ( 118.0294372515226939, 235.5563491861037164, 45.00000000000000000 ) ) ;
#15327 = ORIENTED_EDGE ( 'NONE', *, *, #23166, .F. ) ;
#15328 = VECTOR ( 'NONE', #19176, 1000.000000000000000 ) ;
#15329 = EDGE_CURVE ( 'NONE', #12943, #5065, #15733, .T. ) ;
#15330 = ORIENTED_EDGE ( 'NONE', *, *, #13307, .F. ) ;
#15331 = DIRECTION ( 'NONE',  ( -0.000000000000000000, -0.000000000000000000, -1.000000000000000000 ) ) ;
#15332 = ORIENTED_EDGE ( 'NONE', *, *, #18595, .T. ) ;
#15333 = VERTEX_POINT ( 'NONE', #20309 ) ;
#15334 = CARTESIAN_POINT ( 'NONE',  ( 217.4999999999996305, 258.6181251126050711, 1.387778780781445676E-14 ) ) ;
#15335 = CARTESIAN_POINT ( 'NONE',  ( 157.9999999999999716, 208.9684999699701393, -45.00000000000000000 ) ) ;
#15336 = CARTESIAN_POINT ( 'NONE',  ( 89.82706236705463709, 239.6935390653904392, 16.61376038146385170 ) ) ;
#15337 = EDGE_CURVE ( 'NONE', #962, #2873, #642, .T. ) ;
#15338 = DIRECTION ( 'NONE',  ( 1.000000000000000000, -0.000000000000000000, -0.000000000000000000 ) ) ;
#15339 = DIRECTION ( 'NONE',  ( -0.8916010070293384215, 0.4528218681383106015, 0.000000000000000000 ) ) ;
#15340 = DIRECTION ( 'NONE',  ( -0.000000000000000000, -0.000000000000000000, -1.000000000000000000 ) ) ;
#15341 = LINE ( 'NONE', #527, #12637 ) ;
#15342 = CARTESIAN_POINT ( 'NONE',  ( -227.5045087581038388, 90.32113136995671709, -15.58012468608450440 ) ) ;
#15343 = LINE ( 'NONE', #28241, #3960 ) ;
#15344 = CARTESIAN_POINT ( 'NONE',  ( -274.7382056584871748, -170.0332543031711339, -91.86557292422580190 ) ) ;
#15345 = CARTESIAN_POINT ( 'NONE',  ( 134.9999999999998579, 220.0000000000000284, -84.99999999999997158 ) ) ;
#15346 = FACE_BOUND ( 'NONE', #4377, .T. ) ;
#15347 = CARTESIAN_POINT ( 'NONE',  ( -260.0000000000001137, -157.0000000000000284, -59.99999999999986500 ) ) ;
#15348 = VERTEX_POINT ( 'NONE', #7535 ) ;
#15349 = DIRECTION ( 'NONE',  ( -0.000000000000000000, 0.000000000000000000, -1.000000000000000000 ) ) ;
#15350 = EDGE_CURVE ( 'NONE', #20506, #23733, #2633, .T. ) ;
#15351 = EDGE_CURVE ( 'NONE', #21319, #2405, #16298, .T. ) ;
#15352 = CARTESIAN_POINT ( 'NONE',  ( 163.8948362858342591, 258.6181251126050711, 1.387778780781445676E-14 ) ) ;
#15353 = LINE ( 'NONE', #21659, #2031 ) ;
#15354 = CARTESIAN_POINT ( 'NONE',  ( 108.1035950512893891, 206.7065541617666895, -139.3072807822095740 ) ) ;
#15355 = ORIENTED_EDGE ( 'NONE', *, *, #12335, .F. ) ;
#15356 = APPLICATION_CONTEXT ( 'automotive_design' ) ;
#15357 = CARTESIAN_POINT ( 'NONE',  ( 109.9999999999998863, 259.4346755187099802, -44.02082925162862637 ) ) ;
#15358 = ORIENTED_EDGE ( 'NONE', *, *, #20845, .T. ) ;
#15359 = PRESENTATION_STYLE_ASSIGNMENT (( #8880 ) ) ;
#15360 = ORIENTED_EDGE ( 'NONE', *, *, #7549, .T. ) ;
#15361 = VECTOR ( 'NONE', #12266, 999.9999999999998863 ) ;
#15362 = EDGE_CURVE ( 'NONE', #11671, #13771, #8177, .T. ) ;
#15363 = EDGE_LOOP ( 'NONE', ( #8280, #22951, #9848, #8567 ) ) ;
#15364 = EDGE_LOOP ( 'NONE', ( #28262, #517, #18738, #26117, #9086 ) ) ;
#15365 = AXIS2_PLACEMENT_3D ( 'NONE', #23080, #1098, #27650 ) ;
#15366 = ORIENTED_EDGE ( 'NONE', *, *, #21846, .F. ) ;
#15367 = LINE ( 'NONE', #19797, #5378 ) ;
#15368 = CARTESIAN_POINT ( 'NONE',  ( -160.0000000000000284, 79.99999999999994316, 70.00000000000001421 ) ) ;
#15369 = ADVANCED_FACE ( 'NONE', ( #5924 ), #3906, .F. ) ;
#15370 = CARTESIAN_POINT ( 'NONE',  ( 157.4999999999998579, 48.21056198576756202, -45.00000000000000000 ) ) ;
#15371 = EDGE_CURVE ( 'NONE', #14295, #10017, #11392, .T. ) ;
#15372 = LINE ( 'NONE', #8750, #12596 ) ;
#15373 = CARTESIAN_POINT ( 'NONE',  ( -226.6109647992649059, 62.69877383610198507, 18.44381613006064313 ) ) ;
#15374 = CARTESIAN_POINT ( 'NONE',  ( 209.9999999999988063, -280.0000000000000000, -100.0000000000011084 ) ) ;
#15375 = DIRECTION ( 'NONE',  ( 0.000000000000000000, -1.000000000000000000, 0.000000000000000000 ) ) ;
#15376 = DIRECTION ( 'NONE',  ( 0.000000000000000000, 0.000000000000000000, -1.000000000000000000 ) ) ;
#15377 = CIRCLE ( 'NONE', #4813, 55.86582179324592090 ) ;
#15378 = CARTESIAN_POINT ( 'NONE',  ( 157.4999999999998579, 95.86018712840139244, -45.00000000000000000 ) ) ;
#15379 = DIRECTION ( 'NONE',  ( 1.000000000000000000, -9.102812259465213132E-16, 0.000000000000000000 ) ) ;
#15380 = LINE ( 'NONE', #28134, #12533 ) ;
#15381 = VECTOR ( 'NONE', #1008, 1000.000000000000114 ) ;
#15382 = CARTESIAN_POINT ( 'NONE',  ( -160.0000000000000284, 109.9999999999999432, -70.00000000000001421 ) ) ;
#15383 = DIRECTION ( 'NONE',  ( 0.000000000000000000, 0.000000000000000000, 1.000000000000000000 ) ) ;
#15384 = CARTESIAN_POINT ( 'NONE',  ( -173.2089802904066573, 113.5335206920022273, 28.23679712238971007 ) ) ;
#15385 = CARTESIAN_POINT ( 'NONE',  ( 40.99999999999999289, 6.123233995736766282E-16, -5.000000000000000000 ) ) ;
#15386 = VECTOR ( 'NONE', #18867, 1000.000000000000000 ) ;
#15388 = ORIENTED_EDGE ( 'NONE', *, *, #10548, .T. ) ;
#15387 = VERTEX_POINT ( 'NONE', #25184 ) ;
#15389 = DIRECTION ( 'NONE',  ( -0.000000000000000000, 1.000000000000000000, 1.214306433183764966E-16 ) ) ;
#15390 = CARTESIAN_POINT ( 'NONE',  ( -203.2481855153402250, 92.57460631283319685, -29.78692811926999795 ) ) ;
#15391 = VERTEX_POINT ( 'NONE', #14421 ) ;
#15392 = CONTEXT_DEPENDENT_SHAPE_REPRESENTATION ( #23770, #13274 ) ;
#15393 = VERTEX_POINT ( 'NONE', #27606 ) ;
#15394 = ORIENTED_EDGE ( 'NONE', *, *, #16814, .T. ) ;
#15395 = CARTESIAN_POINT ( 'NONE',  ( 158.0000000000011369, 96.11412463215494029, 45.00000000000000000 ) ) ;
#15396 = CARTESIAN_POINT ( 'NONE',  ( 157.9999999999996874, 269.1575001501400379, 45.00000000000000000 ) ) ;
#15397 = ORIENTED_EDGE ( 'NONE', *, *, #16944, .F. ) ;
#15398 = EDGE_CURVE ( 'NONE', #21416, #5481, #4220, .T. ) ;
#15399 = CIRCLE ( 'NONE', #12187, 16.36034929305424512 ) ;
#15400 = CARTESIAN_POINT ( 'NONE',  ( 93.07270601809125310, 112.9533406970419378, -100.0000000000000142 ) ) ;
#15401 = ADVANCED_FACE ( 'NONE', ( #14282 ), #1334, .F. ) ;
#15402 = LINE ( 'NONE', #26576, #5453 ) ;
#15403 = VERTEX_POINT ( 'NONE', #25464 ) ;
#15404 = CARTESIAN_POINT ( 'NONE',  ( -209.6027893482759907, 89.20079749152587567, 25.07826924335527607 ) ) ;
#15405 = VECTOR ( 'NONE', #11098, 999.9999999999998863 ) ;
#15406 = LINE ( 'NONE', #15119, #9795 ) ;
#15407 = DIRECTION ( 'NONE',  ( -0.000000000000000000, 0.000000000000000000, -1.000000000000000000 ) ) ;
#15408 = CARTESIAN_POINT ( 'NONE',  ( 157.8620484902690180, 200.5745024719774392, -147.6607294899350791 ) ) ;
#15409 = EDGE_LOOP ( 'NONE', ( #8736, #14030, #1080, #19680, #26360 ) ) ;
#15410 = FACE_BOUND ( 'NONE', #26958, .T. ) ;
#15411 = EDGE_CURVE ( 'NONE', #5960, #1808, #16573, .T. ) ;
#15412 = AXIS2_PLACEMENT_3D ( 'NONE', #25588, #12405, #21682 ) ;
#15413 = PLANE ( 'NONE',  #1847 ) ;
#15414 = CARTESIAN_POINT ( 'NONE',  ( 65.00000000000000000, -150.0000000000000568, 64.00000000000002842 ) ) ;
#15415 = DIRECTION ( 'NONE',  ( 0.8916010070299571488, -0.4528218681370922982, 0.000000000000000000 ) ) ;
#15416 = VECTOR ( 'NONE', #26197, 1000.000000000000227 ) ;
#15417 = EDGE_LOOP ( 'NONE', ( #20060, #26450, #17922, #16313 ) ) ;
#15418 = VECTOR ( 'NONE', #21311, 1000.000000000000000 ) ;
#15419 = CARTESIAN_POINT ( 'NONE',  ( -210.3420462306316949, -220.0000000000000853, -108.8941602138125262 ) ) ;
#15420 = EDGE_CURVE ( 'NONE', #24310, #27485, #7944, .T. ) ;
#15421 = LINE ( 'NONE', #24173, #7464 ) ;
#15422 = CARTESIAN_POINT ( 'NONE',  ( -140.5419864827275660, 71.17632247292569048, 82.82905917779648064 ) ) ;
#15423 = EDGE_LOOP ( 'NONE', ( #3555, #9625, #1351, #1437 ) ) ;
#15424 =( NAMED_UNIT ( * ) SI_UNIT ( $, .STERADIAN. ) SOLID_ANGLE_UNIT ( ) );
#15425 = VECTOR ( 'NONE', #6732, 1000.000000000000000 ) ;
#15426 = ORIENTED_EDGE ( 'NONE', *, *, #5035, .F. ) ;
#15427 = DIRECTION ( 'NONE',  ( 0.000000000000000000, -1.000000000000000000, 0.000000000000000000 ) ) ;
#15428 = CARTESIAN_POINT ( 'NONE',  ( -178.3823435749502266, 110.6645840747622032, -30.26113312571055047 ) ) ;
#15429 = ORIENTED_EDGE ( 'NONE', *, *, #2306, .T. ) ;
#15430 = EDGE_CURVE ( 'NONE', #17350, #27032, #25325, .T. ) ;
#15431 = ORIENTED_EDGE ( 'NONE', *, *, #26771, .F. ) ;
#15432 = EDGE_CURVE ( 'NONE', #19721, #9863, #12325, .T. ) ;
#15433 = DIRECTION ( 'NONE',  ( 1.000000000000000000, 0.000000000000000000, 0.000000000000000000 ) ) ;
#15434 = DIRECTION ( 'NONE',  ( 0.8916010070296124246, 0.4528218681377710886, 0.000000000000000000 ) ) ;
#15435 = EDGE_CURVE ( 'NONE', #15494, #23088, #10525, .T. ) ;
#15436 = VERTEX_POINT ( 'NONE', #25739 ) ;
#15437 = ORIENTED_EDGE ( 'NONE', *, *, #6375, .F. ) ;
#15438 = AXIS2_PLACEMENT_3D ( 'NONE', #1804, #14757, #12609 ) ;
#15439 = DIRECTION ( 'NONE',  ( 0.8916010070297846202, -0.4528218681374320265, 0.000000000000000000 ) ) ;
#15440 = CARTESIAN_POINT ( 'NONE',  ( 125.3433571860711453, 242.0587615242396566, -84.99999999999997158 ) ) ;
#15441 = DIRECTION ( 'NONE',  ( 1.000000000000000000, 0.000000000000000000, 0.000000000000000000 ) ) ;
#15442 = CARTESIAN_POINT ( 'NONE',  ( -63.57415822541634043, 75.97823757117562593, 80.00000000000001421 ) ) ;
#15443 = AXIS2_PLACEMENT_3D ( 'NONE', #23349, #23633, #17162 ) ;
#15444 = CARTESIAN_POINT ( 'NONE',  ( -180.0000000000000284, -40.00000000000004974, 98.28427124746191623 ) ) ;
#15445 = CARTESIAN_POINT ( 'NONE',  ( -210.0000000000000853, 59.99999999999993605, -18.66499754458839178 ) ) ;
#15446 = CARTESIAN_POINT ( 'NONE',  ( 155.4185842870420799, 209.3660254037844481, 45.00000000000000000 ) ) ;
#15447 = VERTEX_POINT ( 'NONE', #27747 ) ;
#15448 = CYLINDRICAL_SURFACE ( 'NONE', #10383, 9.999999999999982236 ) ;
#15449 = CARTESIAN_POINT ( 'NONE',  ( 51.56615429303207065, 203.2034914284457159, -15.00000000000000000 ) ) ;
#15450 = DIRECTION ( 'NONE',  ( -0.000000000000000000, -1.000000000000000000, -0.000000000000000000 ) ) ;
#15451 = DIRECTION ( 'NONE',  ( 0.000000000000000000, 0.000000000000000000, -1.000000000000000000 ) ) ;
#15452 = ORIENTED_EDGE ( 'NONE', *, *, #6916, .T. ) ;
#15453 = CARTESIAN_POINT ( 'NONE',  ( 232.4749999999995964, 83.06687458711267880, 30.86484227207694886 ) ) ;
#15454 = ORIENTED_EDGE ( 'NONE', *, *, #12448, .F. ) ;
#15455 = LINE ( 'NONE', #15596, #10222 ) ;
#15456 = CARTESIAN_POINT ( 'NONE',  ( -236.3091765109048481, 68.24607436519741555, -5.736201002603987575 ) ) ;
#15457 = DIRECTION ( 'NONE',  ( -0.5457381880580697286, 0.8379557447115539848, 0.000000000000000000 ) ) ;
#15458 = ORIENTED_EDGE ( 'NONE', *, *, #5945, .T. ) ;
#15459 = CARTESIAN_POINT ( 'NONE',  ( 157.9999999999997442, 249.0945000900840398, -45.00000000000000000 ) ) ;
#15460 = PLANE ( 'NONE',  #17981 ) ;
#15461 = EDGE_LOOP ( 'NONE', ( #7220, #19849, #22560, #9662 ) ) ;
#15462 = AXIS2_PLACEMENT_3D ( 'NONE', #22021, #2328, #6510 ) ;
#15463 = EDGE_CURVE ( 'NONE', #21241, #27621, #12554, .T. ) ;
#15464 = EDGE_CURVE ( 'NONE', #28358, #5554, #23596, .T. ) ;
#15465 = CARTESIAN_POINT ( 'NONE',  ( -212.6581729763558712, 72.57237399018264057, 29.67346677899678298 ) ) ;
#15466 = ORIENTED_EDGE ( 'NONE', *, *, #3391, .F. ) ;
#15467 = LINE ( 'NONE', #13172, #16348 ) ;
#15468 = EDGE_CURVE ( 'NONE', #12778, #27297, #26498, .T. ) ;
#15469 = ORIENTED_EDGE ( 'NONE', *, *, #18656, .F. ) ;
#15470 = VERTEX_POINT ( 'NONE', #7669 ) ;
#15471 = LINE ( 'NONE', #24218, #10833 ) ;
#15472 = ADVANCED_FACE ( 'NONE', ( #16436 ), #23032, .F. ) ;
#15473 = ORIENTED_EDGE ( 'NONE', *, *, #743, .F. ) ;
#15474 = ORIENTED_EDGE ( 'NONE', *, *, #25716, .F. ) ;
#15475 = LINE ( 'NONE', #8574, #20075 ) ;
#15476 = CARTESIAN_POINT ( 'NONE',  ( 98.38712641049259844, 233.7235291372264214, 21.27834768224934692 ) ) ;
#15477 = PRODUCT_RELATED_PRODUCT_CATEGORY ( 'part', '', ( #28144 ) ) ;
#15478 = DIRECTION ( 'NONE',  ( 0.6681556583950127859, 0.7440215159219033536, 0.000000000000000000 ) ) ;
#15479 = LINE ( 'NONE', #6273, #25657 ) ;
#15480 = VECTOR ( 'NONE', #2877, 999.9999999999998863 ) ;
#15481 = DIRECTION ( 'NONE',  ( 0.000000000000000000, 0.000000000000000000, -1.000000000000000000 ) ) ;
#15482 = CARTESIAN_POINT ( 'NONE',  ( -273.6177394993287635, -164.9999999998519797, 86.76313735923795889 ) ) ;
#15483 = DIRECTION ( 'NONE',  ( 1.000000000000000000, 0.000000000000000000, 0.000000000000000000 ) ) ;
#15484 = CARTESIAN_POINT ( 'NONE',  ( 217.4999999999996305, 194.4107529906318064, 288.0938197134494203 ) ) ;
#15485 = CARTESIAN_POINT ( 'NONE',  ( 232.4749999999995964, 83.06687458711267880, 42.86484227207692754 ) ) ;
#15486 = PLANE ( 'NONE',  #15671 ) ;
#15487 = DIRECTION ( 'NONE',  ( 1.000000000000000000, 0.000000000000000000, -0.000000000000000000 ) ) ;
#15488 = DIRECTION ( 'NONE',  ( -0.000000000000000000, -0.000000000000000000, -1.000000000000000000 ) ) ;
#15489 = ORIENTED_EDGE ( 'NONE', *, *, #10407, .T. ) ;
#15490 = CYLINDRICAL_SURFACE ( 'NONE', #21128, 75.00000000000002842 ) ;
#15491 = CARTESIAN_POINT ( 'NONE',  ( -277.2150368962633706, -165.0000000000001137, -90.47363622314027509 ) ) ;
#15492 = CARTESIAN_POINT ( 'NONE',  ( 0.000000000000000000, 330.0000000000000000, -84.99999999999997158 ) ) ;
#15493 = FACE_OUTER_BOUND ( 'NONE', #12996, .T. ) ;
#15494 = VERTEX_POINT ( 'NONE', #18858 ) ;
#15495 = EDGE_CURVE ( 'NONE', #17587, #19047, #23451, .T. ) ;
#15496 = ADVANCED_FACE ( 'NONE', ( #1194 ), #22848, .F. ) ;
#15497 = FACE_OUTER_BOUND ( 'NONE', #11700, .T. ) ;
#15498 = VERTEX_POINT ( 'NONE', #1612 ) ;
#15499 = CARTESIAN_POINT ( 'NONE',  ( -210.0000000000000000, -120.0000000000000711, -100.0000000000000142 ) ) ;
#15500 = ORIENTED_EDGE ( 'NONE', *, *, #17034, .F. ) ;
#15501 = AXIS2_PLACEMENT_3D ( 'NONE', #17078, #28266, #25838 ) ;
#15502 = ORIENTED_EDGE ( 'NONE', *, *, #6864, .F. ) ;
#15503 = EDGE_LOOP ( 'NONE', ( #22781, #25064, #20860, #24630 ) ) ;
#15504 = ORIENTED_EDGE ( 'NONE', *, *, #21111, .T. ) ;
#15505 = ORIENTED_EDGE ( 'NONE', *, *, #27119, .T. ) ;
#15506 = CARTESIAN_POINT ( 'NONE',  ( 158.0000000000005969, 150.7794997898028271, -45.00000000000000000 ) ) ;
#15507 = EDGE_CURVE ( 'NONE', #5621, #22058, #8227, .T. ) ;
#15508 = EDGE_CURVE ( 'NONE', #12180, #23386, #23734, .T. ) ;
#15509 = CARTESIAN_POINT ( 'NONE',  ( 73.69623568533953062, -15.56365422765611051, 45.00000000000000000 ) ) ;
#15510 = UNCERTAINTY_MEASURE_WITH_UNIT (LENGTH_MEASURE( 1.000000000000000082E-05 ), #5050, 'distance_accuracy_value', 'NONE');
#15511 = DIRECTION ( 'NONE',  ( -0.000000000000000000, 0.000000000000000000, 1.000000000000000000 ) ) ;
#15512 = CARTESIAN_POINT ( 'NONE',  ( -210.9349024751243178, 73.41979635535319915, 32.58420779144454826 ) ) ;
#15514 = CIRCLE ( 'NONE', #22846, 9.999999999999996447 ) ;
#15513 = DIRECTION ( 'NONE',  ( -1.000000000000000000, 0.000000000000000000, 0.000000000000000000 ) ) ;
#15515 = CARTESIAN_POINT ( 'NONE',  ( 157.9999999999996305, 284.2047501951820436, 45.00000000000000000 ) ) ;
#15516 = DIRECTION ( 'NONE',  ( 1.000000000000000000, 0.000000000000000000, 0.000000000000000000 ) ) ;
#15517 = LINE ( 'NONE', #22251, #10324 ) ;
#15518 = DIRECTION ( 'NONE',  ( -0.000000000000000000, -0.000000000000000000, -1.000000000000000000 ) ) ;
#15519 = DIRECTION ( 'NONE',  ( -0.000000000000000000, -0.000000000000000000, 1.000000000000000000 ) ) ;
#15520 = ADVANCED_FACE ( 'NONE', ( #15410, #24166, #15126 ), #24299, .T. ) ;
#15521 = EDGE_CURVE ( 'NONE', #5806, #21087, #21459, .T. ) ;
#15522 = CARTESIAN_POINT ( 'NONE',  ( -28.14180936505419695, 127.9576626828097545, 17.52305135179860685 ) ) ;
#15523 = DIRECTION ( 'NONE',  ( -0.000000000000000000, -0.000000000000000000, -1.000000000000000000 ) ) ;
#15524 = DIRECTION ( 'NONE',  ( 1.000000000000000000, 0.000000000000000000, 0.000000000000000000 ) ) ;
#15525 = CARTESIAN_POINT ( 'NONE',  ( 33.10302365956999182, 219.6666220619077876, 12.99999999999999822 ) ) ;
#15527 = VERTEX_POINT ( 'NONE', #21576 ) ;
#15526 = ORIENTED_EDGE ( 'NONE', *, *, #7440, .T. ) ;
#15528 = DIRECTION ( 'NONE',  ( 0.000000000000000000, 0.000000000000000000, -1.000000000000000000 ) ) ;
#15529 = VECTOR ( 'NONE', #262, 1000.000000000000000 ) ;
#15530 = DIRECTION ( 'NONE',  ( 0.000000000000000000, 0.000000000000000000, -1.000000000000000000 ) ) ;
#15531 = VERTEX_POINT ( 'NONE', #4043 ) ;
#15532 = EDGE_LOOP ( 'NONE', ( #4100, #14677, #10756, #18570 ) ) ;
#15533 = ORIENTED_EDGE ( 'NONE', *, *, #17413, .F. ) ;
#15534 = AXIS2_PLACEMENT_3D ( 'NONE', #9446, #13909, #4969 ) ;
#15535 = CARTESIAN_POINT ( 'NONE',  ( 158.0000000000014779, 65.51174953456337846, 45.00000000000000000 ) ) ;
#15536 = CARTESIAN_POINT ( 'NONE',  ( -151.6073178449016154, 124.1689584723159072, 19.47232524047854341 ) ) ;
#15537 = VECTOR ( 'NONE', #19283, 1000.000000000000000 ) ;
#15538 = ORIENTED_EDGE ( 'NONE', *, *, #799, .F. ) ;
#15539 = LINE ( 'NONE', #17533, #5822 ) ;
#15540 = ADVANCED_FACE ( 'NONE', ( #4463 ), #28333, .F. ) ;
#15541 = CARTESIAN_POINT ( 'NONE',  ( 157.9999999999996589, 281.1890001801680796, -45.00000000000000000 ) ) ;
#15542 = ORIENTED_EDGE ( 'NONE', *, *, #9744, .T. ) ;
#15543 = CARTESIAN_POINT ( 'NONE',  ( -221.2146732495352239, 88.15369072822400653, 15.78728978121136883 ) ) ;
#15544 = DIRECTION ( 'NONE',  ( -0.000000000000000000, -0.000000000000000000, -1.000000000000000000 ) ) ;
#15545 = CARTESIAN_POINT ( 'NONE',  ( 282.4999999999996589, 19.41075299063184900, 87.99671038392668265 ) ) ;
#15546 = CARTESIAN_POINT ( 'NONE',  ( 159.3469981926682806, 202.4713331616098912, -139.8040206391607398 ) ) ;
#15547 = AXIS2_PLACEMENT_3D ( 'NONE', #11128, #9408, #15882 ) ;
#15548 = VERTEX_POINT ( 'NONE', #4606 ) ;
#15549 = PLANE ( 'NONE',  #3574 ) ;
#15550 = CIRCLE ( 'NONE', #1305, 10.00000000000000888 ) ;
#15551 = LINE ( 'NONE', #9221, #11965 ) ;
#15552 = FACE_OUTER_BOUND ( 'NONE', #7402, .T. ) ;
#15553 = FACE_OUTER_BOUND ( 'NONE', #2067, .T. ) ;
#15554 = ORIENTED_EDGE ( 'NONE', *, *, #27528, .T. ) ;
#15555 = EDGE_CURVE ( 'NONE', #20391, #11099, #6776, .T. ) ;
#15556 = CARTESIAN_POINT ( 'NONE',  ( -212.2419371577844913, -220.0000000000001137, -105.4110757242456771 ) ) ;
#15557 = ADVANCED_FACE ( 'NONE', ( #2452 ), #15549, .F. ) ;
#15558 = CARTESIAN_POINT ( 'NONE',  ( 157.9999999999999432, 211.4763749774776045, 45.00000000000000000 ) ) ;
#15559 = CARTESIAN_POINT ( 'NONE',  ( -141.7923270636435404, 70.43557993099105374, 82.87231033183468298 ) ) ;
#15560 = EDGE_LOOP ( 'NONE', ( #12745, #1624, #20922, #7127 ) ) ;
#15561 = EDGE_CURVE ( 'NONE', #16958, #24084, #28170, .T. ) ;
#15562 = ORIENTED_EDGE ( 'NONE', *, *, #23058, .T. ) ;
#15563 = CARTESIAN_POINT ( 'NONE',  ( 157.9999999999998579, 219.0000000000000284, 45.00000000000000000 ) ) ;
#15564 = CIRCLE ( 'NONE', #428, 17.46154499483315448 ) ;
#15565 = CARTESIAN_POINT ( 'NONE',  ( 2.399999999999999911, 1.249999999999999556, 7.582700855991164168 ) ) ;
#15566 = ORIENTED_EDGE ( 'NONE', *, *, #24570, .F. ) ;
#15567 = VECTOR ( 'NONE', #24581, 1000.000000000000000 ) ;
#15568 = EDGE_LOOP ( 'NONE', ( #7893, #7952, #5306, #14888 ) ) ;
#15569 = DIRECTION ( 'NONE',  ( 0.000000000000000000, 0.000000000000000000, 1.000000000000000000 ) ) ;
#15570 = VECTOR ( 'NONE', #13334, 1000.000000000000114 ) ;
#15571 = CARTESIAN_POINT ( 'NONE',  ( 3.660298066448477439, -2.383854334960948229, 45.00000000000000000 ) ) ;
#15572 = ORIENTED_EDGE ( 'NONE', *, *, #17811, .T. ) ;
#15573 = ORIENTED_EDGE ( 'NONE', *, *, #206, .T. ) ;
#15574 = CARTESIAN_POINT ( 'NONE',  ( -17.91222884894589029, 128.7240434152827788, 17.19583536164714488 ) ) ;
#15575 = LINE ( 'NONE', #6376, #14940 ) ;
#15576 = FACE_OUTER_BOUND ( 'NONE', #26939, .T. ) ;
#15577 = CARTESIAN_POINT ( 'NONE',  ( 81.39309752945497678, 249.3891174404998594, 45.00000000000000000 ) ) ;
#15578 = DIRECTION ( 'NONE',  ( 0.8916010070293515222, 0.4528218681382848443, 0.000000000000000000 ) ) ;
#15579 = CARTESIAN_POINT ( 'NONE',  ( -266.6560114757872952, -170.8199632925098115, 104.6399347438232894 ) ) ;
#15580 = LINE ( 'NONE', #17866, #9154 ) ;
#15581 = EDGE_LOOP ( 'NONE', ( #861, #1930, #24612, #21193 ) ) ;
#15582 = AXIS2_PLACEMENT_3D ( 'NONE', #12383, #8052, #18688 ) ;
#15583 = LINE ( 'NONE', #6384, #10461 ) ;
#15584 = AXIS2_PLACEMENT_3D ( 'NONE', #13041, #21788, #21639 ) ;
#15585 = ADVANCED_FACE ( 'NONE', ( #6206 ), #28025, .F. ) ;
#15586 = LINE ( 'NONE', #21897, #10185 ) ;
#15587 = DIRECTION ( 'NONE',  ( 1.000000000000000000, -1.850371707708594366E-15, 0.000000000000000000 ) ) ;
#15588 = DIRECTION ( 'NONE',  ( -0.000000000000000000, -0.000000000000000000, -1.000000000000000000 ) ) ;
#15589 = ORIENTED_EDGE ( 'NONE', *, *, #12617, .F. ) ;
#15590 = EDGE_CURVE ( 'NONE', #16161, #24580, #20092, .T. ) ;
#15591 = FACE_OUTER_BOUND ( 'NONE', #22196, .T. ) ;
#15592 = ADVANCED_FACE ( 'NONE', ( #22000 ), #14986, .F. ) ;
#15593 = AXIS2_PLACEMENT_3D ( 'NONE', #12456, #8416, #17174 ) ;
#15594 = ORIENTED_EDGE ( 'NONE', *, *, #4998, .T. ) ;
#15595 = EDGE_CURVE ( 'NONE', #11364, #1874, #8788, .T. ) ;
#15596 = CARTESIAN_POINT ( 'NONE',  ( 157.4999999999996874, 271.4114376538935289, -45.00000000000000000 ) ) ;
#15597 = DIRECTION ( 'NONE',  ( 0.9784193629480814058, 0.2066290158914539099, -0.000000000000000000 ) ) ;
#15598 = CARTESIAN_POINT ( 'NONE',  ( 140.3821234321421230, 249.5134143970365983, -142.3407963099403162 ) ) ;
#15599 = ORIENTED_EDGE ( 'NONE', *, *, #22025, .T. ) ;
#15600 = DIRECTION ( 'NONE',  ( 1.000000000000000000, -0.000000000000000000, -0.000000000000000000 ) ) ;
#15601 = LINE ( 'NONE', #23927, #6511 ) ;
#15602 = ORIENTED_EDGE ( 'NONE', *, *, #18053, .F. ) ;
#15603 = AXIS2_PLACEMENT_3D ( 'NONE', #12474, #16637, #19203 ) ;
#15604 = CARTESIAN_POINT ( 'NONE',  ( -208.5121489769019547, 74.88284981659903394, 38.34302025979879858 ) ) ;
#15605 = ORIENTED_EDGE ( 'NONE', *, *, #10979, .F. ) ;
#15606 = CARTESIAN_POINT ( 'NONE',  ( -277.2150368962633706, -170.0000000000001137, 90.47363622314043141 ) ) ;
#15607 = ORIENTED_EDGE ( 'NONE', *, *, #18568, .F. ) ;
#15608 = ORIENTED_EDGE ( 'NONE', *, *, #10522, .F. ) ;
#15609 = DIRECTION ( 'NONE',  ( -0.000000000000000000, 0.000000000000000000, -1.000000000000000000 ) ) ;
#15610 = EDGE_LOOP ( 'NONE', ( #13822, #20326, #19264, #23036 ) ) ;
#15611 = CIRCLE ( 'NONE', #22028, 1.999999999999994893 ) ;
#15612 = VERTEX_POINT ( 'NONE', #26023 ) ;
#15613 = ORIENTED_EDGE ( 'NONE', *, *, #26021, .T. ) ;
#15614 = CARTESIAN_POINT ( 'NONE',  ( -223.0228900756071653, 134.9178336739567499, 12.97939780113086705 ) ) ;
#15615 = CARTESIAN_POINT ( 'NONE',  ( 94.04374108504261187, 240.3974664687521567, 8.346404539543760492 ) ) ;
#15616 = AXIS2_PLACEMENT_3D ( 'NONE', #14519, #16946, #27841 ) ;
#15617 = CARTESIAN_POINT ( 'NONE',  ( -254.3350114625770289, -91.18033988749901653, 16.36034929305424512 ) ) ;
#15618 = DIRECTION ( 'NONE',  ( 0.000000000000000000, 0.000000000000000000, -1.000000000000000000 ) ) ;
#15619 = EDGE_CURVE ( 'NONE', #2501, #11684, #23917, .T. ) ;
#15620 = DIRECTION ( 'NONE',  ( 1.000000000000000000, 0.000000000000000000, 0.000000000000000000 ) ) ;
#15621 = EDGE_CURVE ( 'NONE', #20045, #7328, #22396, .T. ) ;
#15622 = DIRECTION ( 'NONE',  ( -0.9985600561963485777, 0.05364526231779760679, 0.000000000000000000 ) ) ;
#15623 = FACE_OUTER_BOUND ( 'NONE', #22697, .T. ) ;
#15624 = DIRECTION ( 'NONE',  ( 0.7071067811865474617, 0.000000000000000000, -0.7071067811865474617 ) ) ;
#15625 = CARTESIAN_POINT ( 'NONE',  ( 79.99999999999994316, -70.00000000000002842, 25.00000000000000000 ) ) ;
#15626 = CARTESIAN_POINT ( 'NONE',  ( 157.4999999999996874, 271.4114376538935289, 45.00000000000000000 ) ) ;
#15627 = FACE_OUTER_BOUND ( 'NONE', #7429, .T. ) ;
#15628 = LINE ( 'NONE', #251, #7026 ) ;
#15629 = ORIENTED_EDGE ( 'NONE', *, *, #26461, .F. ) ;
#15630 = DIRECTION ( 'NONE',  ( -0.000000000000000000, -0.000000000000000000, -1.000000000000000000 ) ) ;
#15631 = EDGE_CURVE ( 'NONE', #12077, #9740, #26308, .T. ) ;
#15632 = AXIS2_PLACEMENT_3D ( 'NONE', #9681, #2924, #7532 ) ;
#15633 = EDGE_CURVE ( 'NONE', #26492, #16142, #26886, .T. ) ;
#15634 = LINE ( 'NONE', #18211, #15140 ) ;
#15635 = CARTESIAN_POINT ( 'NONE',  ( 157.9999999999996874, 271.1575001501400379, 45.00000000000000000 ) ) ;
#15636 = DIRECTION ( 'NONE',  ( 1.000000000000000000, 1.764238432794959761E-15, 0.000000000000000000 ) ) ;
#15637 = VERTEX_POINT ( 'NONE', #18267 ) ;
#15638 = VECTOR ( 'NONE', #24375, 1000.000000000000000 ) ;
#15639 = CARTESIAN_POINT ( 'NONE',  ( 107.7348956500412385, 246.7603209947076834, -33.46154240484388964 ) ) ;
#15640 = VERTEX_POINT ( 'NONE', #7355 ) ;
#15641 = CARTESIAN_POINT ( 'NONE',  ( 4.489296788125576754, 138.9197681802679369, -13.09539705602191972 ) ) ;
#15642 = EDGE_LOOP ( 'NONE', ( #22843, #7756, #4700, #10125 ) ) ;
#15643 = ORIENTED_EDGE ( 'NONE', *, *, #3281, .T. ) ;
#15644 = ORIENTED_EDGE ( 'NONE', *, *, #28361, .F. ) ;
#15645 = VERTEX_POINT ( 'NONE', #15845 ) ;
#15646 = ORIENTED_EDGE ( 'NONE', *, *, #23956, .T. ) ;
#15647 = DIRECTION ( 'NONE',  ( 0.000000000000000000, -1.000000000000000000, 0.000000000000000000 ) ) ;
#15648 = DIRECTION ( 'NONE',  ( -0.000000000000000000, -0.7071067811865514585, -0.7071067811865435759 ) ) ;
#15649 = DIRECTION ( 'NONE',  ( -0.000000000000000000, -1.000000000000000000, -0.000000000000000000 ) ) ;
#15650 = TOROIDAL_SURFACE ( 'NONE', #10148, 7.509856658345970715, 10.53396790234564762 ) ;
#15651 = DIRECTION ( 'NONE',  ( 0.000000000000000000, 0.000000000000000000, 1.000000000000000000 ) ) ;
#15652 = EDGE_CURVE ( 'NONE', #689, #14759, #745, .T. ) ;
#15653 = CARTESIAN_POINT ( 'NONE',  ( 134.0000000000000853, 196.9999999999997442, 45.00000000000000000 ) ) ;
#15654 = VECTOR ( 'NONE', #12663, 1000.000000000000000 ) ;
#15655 = CARTESIAN_POINT ( 'NONE',  ( -214.3579997887104298, 72.01340221155322752, 27.44224251620622113 ) ) ;
#15656 = LINE ( 'NONE', #26844, #22945 ) ;
#15657 = ADVANCED_FACE ( 'NONE', ( #27160 ), #321, .F. ) ;
#15658 = FACE_OUTER_BOUND ( 'NONE', #15610, .T. ) ;
#15659 = LINE ( 'NONE', #7005, #17702 ) ;
#15660 = DIRECTION ( 'NONE',  ( 1.541976423090495387E-16, -1.000000000000000000, 0.000000000000000000 ) ) ;
#15661 = DIRECTION ( 'NONE',  ( 0.000000000000000000, 0.000000000000000000, -1.000000000000000000 ) ) ;
#15662 = LINE ( 'NONE', #24408, #14828 ) ;
#15663 = CARTESIAN_POINT ( 'NONE',  ( -5.301150576437182238, 133.7253806968913636, 14.04417438168983345 ) ) ;
#15664 = DIRECTION ( 'NONE',  ( 1.000000000000000000, 0.000000000000000000, 0.000000000000000000 ) ) ;
#15665 = LINE ( 'NONE', #2282, #19779 ) ;
#15666 = DIRECTION ( 'NONE',  ( -0.3102637045530588500, 0.9506505318133535720, 0.000000000000000000 ) ) ;
#15668 = ORIENTED_EDGE ( 'NONE', *, *, #18816, .T. ) ;
#15667 = ORIENTED_EDGE ( 'NONE', *, *, #3401, .F. ) ;
#15669 = DIRECTION ( 'NONE',  ( -0.000000000000000000, 1.214306433183764720E-16, -1.000000000000000000 ) ) ;
#15670 = EDGE_CURVE ( 'NONE', #7590, #22406, #2601, .T. ) ;
#15671 = AXIS2_PLACEMENT_3D ( 'NONE', #11464, #4681, #13190 ) ;
#15672 = DIRECTION ( 'NONE',  ( -1.000000000000000000, 0.000000000000000000, 0.000000000000000000 ) ) ;
#15673 = CARTESIAN_POINT ( 'NONE',  ( -207.2829329158516316, 90.24556741685469774, -26.81980500862954031 ) ) ;
#15674 = EDGE_LOOP ( 'NONE', ( #13739, #15605, #8198, #2616, #5274, #11575, #6224, #25349, #19252, #9655, #9871, #9938, #27790, #6200, #7723, #27827, #24119, #25089, #25758, #24039, #1705, #24458, #10967, #21982, #16935, #697, #28385, #26971, #16591, #2163, #20677, #26533, #15705, #1557, #26610, #1282, #12923, #20531, #9800, #16245, #3312, #14955, #965, #27219, #6282, #2719, #15934, #26907, #940, #26098, #2150, #4070, #7683, #1494, #13866, #16320, #18463, #17670, #18209, #8465, #15644, #3002, #9987, #13404, #21314, #12403, #18466, #8602, #3492, #24085, #23796, #151, #1278, #7716, #16621, #19332, #20618, #19930, #9429, #5345, #4140, #24314, #1314, #7473, #28345, #12717, #9306, #21275, #28260, #27924, #16712, #17066, #28113, #18151, #15270, #14534, #23183, #9943, #14670, #23370, #1458, #6929, #18024, #8091, #12117, #13846, #11182, #21847, #23860, #21559, #16631, #9242, #18310, #16571, #2689, #26565, #19625, #4282, #2284, #16181, #14123, #21381, #22771, #11219, #5443, #12534, #405, #2252, #7753, #26346, #26171, #13686, #20221, #2222, #306, #7068, #3736, #20932, #23865, #5561, #16373, #19172, #4888, #21948, #7957, #6148, #24384, #6622, #12298, #18773, #14900, #730, #7741, #19414, #20181, #10503, #2039, #12222, #26490, #26934, #6682, #23364, #23794, #17820, #22921, #7538, #13636, #2789, #21747, #24080, #18591, #5837, #15164, #17890, #8920, #25595, #21775, #18913, #19435, #21600, #23326, #19477, #162, #28180, #22984, #15760, #13341, #11540, #798, #6901, #26081, #22491, #19591, #2926, #18114, #11876, #20187, #14470, #20398, #7364, #21875, #14460, #6506, #22980, #10615, #15794, #24680, #11552, #23440, #1104, #10600, #13002, #8598, #9703, #25858, #1584, #3587, #87, #9234, #17204, #930, #9843, #15719, #18952, #16545, #23725, #6945, #5130, #16216, #21951, #25024, #16801, #4158, #3559, #9171, #4870, #11507, #27045, #1589, #27978, #17387, #24600, #13981, #16560, #14576, #14299, #7271, #9298, #18660, #28037, #28188, #20101, #27247, #2185, #5809, #18485, #13551, #6651, #24708, #18078, #17878, #4558, #12469, #9553, #22597, #8914, #8200, #11043, #7813, #3619, #9392, #7299, #14702, #17525, #28397, #24425, #19094, #4771, #28327, #12029, #11511, #22698, #7785, #25925, #18292, #13295, #1035, #8312, #18443, #890, #21553, #18564, #12552, #14642, #7436, #17210, #3469, #19654, #15110, #17608 ) ) ;
#15675 = ORIENTED_EDGE ( 'NONE', *, *, #23333, .T. ) ;
#15676 = ORIENTED_EDGE ( 'NONE', *, *, #20866, .F. ) ;
#15677 = AXIS2_PLACEMENT_3D ( 'NONE', #3026, #14107, #22857 ) ;
#15678 = DIRECTION ( 'NONE',  ( -0.000000000000000000, -0.000000000000000000, -1.000000000000000000 ) ) ;
#15679 = CARTESIAN_POINT ( 'NONE',  ( -158.6464230094932191, 121.2366000616820116, 20.46992577562846094 ) ) ;
#15680 = VERTEX_POINT ( 'NONE', #7496 ) ;
#15681 = ORIENTED_EDGE ( 'NONE', *, *, #22756, .F. ) ;
#15682 = ADVANCED_FACE ( 'NONE', ( #24873 ), #16123, .T. ) ;
#15683 = FACE_OUTER_BOUND ( 'NONE', #20542, .T. ) ;
#15684 = LINE ( 'NONE', #9065, #25627 ) ;
#15685 = ORIENTED_EDGE ( 'NONE', *, *, #21939, .T. ) ;
#15686 = CARTESIAN_POINT ( 'NONE',  ( -205.2899939696512206, 91.43266760401971283, 27.40424638492752862 ) ) ;
#15687 = CARTESIAN_POINT ( 'NONE',  ( 158.0000000000007674, 131.2243747372535267, 45.00000000000000000 ) ) ;
#15688 = EDGE_CURVE ( 'NONE', #5089, #11585, #14106, .T. ) ;
#15689 = DIRECTION ( 'NONE',  ( 1.000000000000000000, 0.000000000000000000, 0.000000000000000000 ) ) ;
#15690 = VECTOR ( 'NONE', #1762, 1000.000000000000000 ) ;
#15691 = CARTESIAN_POINT ( 'NONE',  ( 158.4255425807448603, 201.2564237786189949, -148.9655004847909936 ) ) ;
#15692 = CARTESIAN_POINT ( 'NONE',  ( -196.2821818994568162, 62.43869624199520985, -34.70549414534111321 ) ) ;
#15693 = VECTOR ( 'NONE', #23820, 1000.000000000000000 ) ;
#15694 = EDGE_LOOP ( 'NONE', ( #11373, #9737, #374, #2034 ) ) ;
#15695 = CARTESIAN_POINT ( 'NONE',  ( 217.4999999999996305, 133.0668745871126930, 30.86484227207697018 ) ) ;
#15696 = CARTESIAN_POINT ( 'NONE',  ( -226.9194714820147567, 131.5555516077983782, -12.99999999956374452 ) ) ;
#15697 = CARTESIAN_POINT ( 'NONE',  ( -277.2150368962633706, -237.2150368962634559, -89.99999999999985789 ) ) ;
#15698 = LINE ( 'NONE', #4334, #27255 ) ;
#15699 = ORIENTED_EDGE ( 'NONE', *, *, #8265, .T. ) ;
#15700 = PLANE ( 'NONE',  #25636 ) ;
#15701 = EDGE_CURVE ( 'NONE', #12426, #17181, #6915, .T. ) ;
#15702 = ADVANCED_FACE ( 'NONE', ( #11679 ), #17834, .F. ) ;
#15703 = DIRECTION ( 'NONE',  ( -4.625929269271485914E-16, 1.000000000000000000, 0.000000000000000000 ) ) ;
#15704 = CARTESIAN_POINT ( 'NONE',  ( -139.1329441303325325, 71.54464929955096864, 82.80879831960034210 ) ) ;
#15705 = ORIENTED_EDGE ( 'NONE', *, *, #1003, .F. ) ;
#15706 = SHAPE_REPRESENTATION_RELATIONSHIP ( 'NONE' , 'NONE' ,  #14145, #24247 ) ;
#15707 = VERTEX_POINT ( 'NONE', #20554 ) ;
#15708 = VECTOR ( 'NONE', #5189, 1000.000000000000000 ) ;
#15709 = LINE ( 'NONE', #2324, #6056 ) ;
#15710 = CARTESIAN_POINT ( 'NONE',  ( -199.1252820381085655, 96.45000389891778525, -30.47981965597484688 ) ) ;
#15711 = ORIENTED_EDGE ( 'NONE', *, *, #27341, .F. ) ;
#15712 = AXIS2_PLACEMENT_3D ( 'NONE', #98, #385, #7279 ) ;
#15714 = EDGE_CURVE ( 'NONE', #17167, #15103, #20415, .T. ) ;
#15713 = ORIENTED_EDGE ( 'NONE', *, *, #11045, .T. ) ;
#15715 = DIRECTION ( 'NONE',  ( 0.8916010070298049373, -0.4528218681373920584, 0.000000000000000000 ) ) ;
#15716 = COLOUR_RGB ( '',0.7921568627450980005, 0.8196078431372548767, 0.9333333333333333481 ) ;
#15717 = LINE ( 'NONE', #28326, #19833 ) ;
#15718 = ORIENTED_EDGE ( 'NONE', *, *, #18436, .T. ) ;
#15719 = ORIENTED_EDGE ( 'NONE', *, *, #9125, .F. ) ;
#15720 = EDGE_CURVE ( 'NONE', #4224, #16662, #12353, .T. ) ;
#15721 = CARTESIAN_POINT ( 'NONE',  ( -11.21207136966835449, 130.1511864905693017, 16.65378689143514634 ) ) ;
#15722 = EDGE_CURVE ( 'NONE', #24374, #5556, #3025, .T. ) ;
#15723 = CARTESIAN_POINT ( 'NONE',  ( 104.9999999999998579, 220.0000000000000284, -122.9999999999999574 ) ) ;
#15724 = ADVANCED_FACE ( 'NONE', ( #879 ), #25014, .F. ) ;
#15725 = DIRECTION ( 'NONE',  ( -0.000000000000000000, -0.000000000000000000, -1.000000000000000000 ) ) ;
#15726 = CARTESIAN_POINT ( 'NONE',  ( -20.10010832150799587, 128.4146997938364052, -17.32638360930989663 ) ) ;
#15727 = CARTESIAN_POINT ( 'NONE',  ( -5.421010862427522170E-17, -1.250000000000000444, 6.997769477110050929 ) ) ;
#15728 = AXIS2_PLACEMENT_3D ( 'NONE', #13786, #16081, #26009 ) ;
#15729 = CARTESIAN_POINT ( 'NONE',  ( -209.5848674449188422, 66.48010988065568938, -33.34549737723507690 ) ) ;
#15730 = CARTESIAN_POINT ( 'NONE',  ( 109.0192378864665557, 205.0000000000002842, -151.0000000000000284 ) ) ;
#15731 = ORIENTED_EDGE ( 'NONE', *, *, #23804, .F. ) ;
#15732 = AXIS2_PLACEMENT_3D ( 'NONE', #6954, #20029, #6811 ) ;
#15733 = LINE ( 'NONE', #24482, #18277 ) ;
#15734 = DIRECTION ( 'NONE',  ( 0.4528218681383106015, -0.8916010070293384215, 0.000000000000000000 ) ) ;
#15736 = DIRECTION ( 'NONE',  ( -1.000000000000000000, 0.000000000000000000, 0.000000000000000000 ) ) ;
#15735 = CIRCLE ( 'NONE', #24912, 5.999999999999991118 ) ;
#15737 = CARTESIAN_POINT ( 'NONE',  ( 109.9999999999999432, 110.0000000000000142, 70.00000000000001421 ) ) ;
#15738 = VERTEX_POINT ( 'NONE', #15695 ) ;
#15739 = DIRECTION ( 'NONE',  ( 1.000000000000000000, 0.000000000000000000, 0.000000000000000000 ) ) ;
#15740 = AXIS2_PLACEMENT_3D ( 'NONE', #26861, #11360, #16102 ) ;
#15741 = ORIENTED_EDGE ( 'NONE', *, *, #5146, .F. ) ;
#15742 = FACE_OUTER_BOUND ( 'NONE', #12282, .T. ) ;
#15743 = CARTESIAN_POINT ( 'NONE',  ( -233.4149848405407965, 66.33036726544322903, -6.308275885109299708 ) ) ;
#15744 = CARTESIAN_POINT ( 'NONE',  ( 157.9999999999997442, 253.6023750975910502, -45.00000000000000000 ) ) ;
#15745 = ORIENTED_EDGE ( 'NONE', *, *, #3191, .F. ) ;
#15746 = DIRECTION ( 'NONE',  ( -0.000000000000000000, -1.000000000000000000, -0.000000000000000000 ) ) ;
#15747 = CARTESIAN_POINT ( 'NONE',  ( 147.1752285801741493, 235.8670668058244644, 45.00000000000000000 ) ) ;
#15748 = ADVANCED_FACE ( 'NONE', ( #24446 ), #26737, .F. ) ;
#15749 = EDGE_LOOP ( 'NONE', ( #13174, #9988, #8821, #5595 ) ) ;
#15750 = CARTESIAN_POINT ( 'NONE',  ( 134.9999999999998579, 220.0000000000000284, 90.00000000000002842 ) ) ;
#15751 = EDGE_LOOP ( 'NONE', ( #1588, #5823, #5137, #13070 ) ) ;
#15752 = PLANE ( 'NONE',  #21371 ) ;
#15753 = EDGE_LOOP ( 'NONE', ( #12524, #16521, #18362, #13207 ) ) ;
#15754 = AXIS2_PLACEMENT_3D ( 'NONE', #6372, #16740, #8254 ) ;
#15755 = EDGE_LOOP ( 'NONE', ( #14479, #26862, #27403, #23873 ) ) ;
#15756 = CARTESIAN_POINT ( 'NONE',  ( 432.4999999999996589, 44.41075299063185611, 75.99342076785332267 ) ) ;
#15757 = ORIENTED_EDGE ( 'NONE', *, *, #25671, .F. ) ;
#15758 = VECTOR ( 'NONE', #28215, 1000.000000000000000 ) ;
#15759 = ORIENTED_EDGE ( 'NONE', *, *, #5831, .F. ) ;
#15760 = ORIENTED_EDGE ( 'NONE', *, *, #20404, .F. ) ;
#15761 = VECTOR ( 'NONE', #15056, 1000.000000000000000 ) ;
#15762 = EDGE_CURVE ( 'NONE', #18196, #2545, #22434, .T. ) ;
#15763 = CARTESIAN_POINT ( 'NONE',  ( 105.7038310726827888, 247.5990904218997173, 23.20200675067667362 ) ) ;
#15764 = VECTOR ( 'NONE', #401, 1000.000000000000000 ) ;
#15765 = EDGE_CURVE ( 'NONE', #27472, #15738, #23329, .T. ) ;
#15766 = DIRECTION ( 'NONE',  ( -1.000000000000000000, 0.000000000000000000, 0.000000000000000000 ) ) ;
#15767 = LINE ( 'NONE', #27088, #23406 ) ;
#15768 = FACE_OUTER_BOUND ( 'NONE', #5773, .T. ) ;
#15769 = FACE_OUTER_BOUND ( 'NONE', #23054, .T. ) ;
#15770 = CARTESIAN_POINT ( 'NONE',  ( -63.57415822541634043, 75.97823757117562593, 100.0000000000000000 ) ) ;
#15771 = CARTESIAN_POINT ( 'NONE',  ( -207.5044420441007276, 75.59897387903043864, -45.00000000000000000 ) ) ;
#15772 = DIRECTION ( 'NONE',  ( -0.8916010070297852863, -0.4528218681374307497, 0.000000000000000000 ) ) ;
#15773 = DIRECTION ( 'NONE',  ( 0.000000000000000000, 0.000000000000000000, 1.000000000000000000 ) ) ;
#15774 = CARTESIAN_POINT ( 'NONE',  ( -290.0000000000001705, -165.0000000000001137, -59.99999999999986500 ) ) ;
#15775 = DIRECTION ( 'NONE',  ( 0.000000000000000000, -1.000000000000000000, -1.214306433183764966E-16 ) ) ;
#15776 = EDGE_LOOP ( 'NONE', ( #9196, #4561, #16824, #13676 ) ) ;
#15777 = VECTOR ( 'NONE', #3716, 1000.000000000000000 ) ;
#15778 = DIRECTION ( 'NONE',  ( 1.000000000000000000, 0.000000000000000000, -0.000000000000000000 ) ) ;
#15779 = CIRCLE ( 'NONE', #3366, 30.00000000000000000 ) ;
#15780 = EDGE_CURVE ( 'NONE', #19657, #15896, #22581, .T. ) ;
#15781 = LINE ( 'NONE', #9302, #2738 ) ;
#15782 = CARTESIAN_POINT ( 'NONE',  ( -2.081668171172168513E-14, 79.99999999999998579, 70.00000000000001421 ) ) ;
#15783 = FACE_OUTER_BOUND ( 'NONE', #10965, .T. ) ;
#15784 = AXIS2_PLACEMENT_3D ( 'NONE', #23494, #5965, #6388 ) ;
#15785 = VERTEX_POINT ( 'NONE', #7771 ) ;
#15786 = CARTESIAN_POINT ( 'NONE',  ( 109.9760533923165156, 258.8696700914497342, -43.04221176959693196 ) ) ;
#15787 = EDGE_LOOP ( 'NONE', ( #5626, #3566, #13379, #21596 ) ) ;
#15788 = ADVANCED_FACE ( 'NONE', ( #1579 ), #14660, .T. ) ;
#15789 = ORIENTED_EDGE ( 'NONE', *, *, #2856, .F. ) ;
#15790 = EDGE_LOOP ( 'NONE', ( #26219, #23682, #7651, #5810, #10530, #6686, #21372, #27683, #16424, #28104, #22585, #7553, #5120, #629, #18141 ) ) ;
#15791 = ORIENTED_EDGE ( 'NONE', *, *, #20262, .T. ) ;
#15792 = ORIENTED_EDGE ( 'NONE', *, *, #22889, .F. ) ;
#15793 = EDGE_CURVE ( 'NONE', #18588, #18153, #19105, .T. ) ;
#15794 = ORIENTED_EDGE ( 'NONE', *, *, #18796, .F. ) ;
#15795 = CARTESIAN_POINT ( 'NONE',  ( -47.46824071874176099, 132.2249976274591177, 14.48593008886889244 ) ) ;
#15796 = AXIS2_PLACEMENT_3D ( 'NONE', #6095, #19454, #25911 ) ;
#15797 = DIRECTION ( 'NONE',  ( -0.8916010070299679180, -0.4528218681370710375, 0.000000000000000000 ) ) ;
#15798 = FACE_OUTER_BOUND ( 'NONE', #6894, .T. ) ;
#15799 = EDGE_CURVE ( 'NONE', #20330, #5281, #12238, .T. ) ;
#15800 = EDGE_CURVE ( 'NONE', #3728, #12262, #12378, .T. ) ;
#15801 = CARTESIAN_POINT ( 'NONE',  ( 79.99999999999990052, 230.0000000000000284, -45.00000000000000000 ) ) ;
#15802 = VECTOR ( 'NONE', #5468, 1000.000000000000000 ) ;
#15803 = UNCERTAINTY_MEASURE_WITH_UNIT (LENGTH_MEASURE( 1.000000000000000082E-05 ), #5516, 'distance_accuracy_value', 'NONE');
#15804 = CARTESIAN_POINT ( 'NONE',  ( 367.4999999999996021, 44.41075299063185611, -75.00000000000001421 ) ) ;
#15805 = CARTESIAN_POINT ( 'NONE',  ( -217.4092282431682577, 59.59925738963178077, 26.62835594396387506 ) ) ;
#15806 = CARTESIAN_POINT ( 'NONE',  ( 158.0000000000006821, 140.7479997597746433, -45.00000000000000000 ) ) ;
#15807 = CARTESIAN_POINT ( 'NONE',  ( 134.9999999999998579, 220.0000000000000284, 90.00000000000002842 ) ) ;
#15808 = FACE_OUTER_BOUND ( 'NONE', #6444, .T. ) ;
#15809 = PLANE ( 'NONE',  #16303 ) ;
#15811 = B_SPLINE_CURVE_WITH_KNOTS ( 'NONE', 3,
 ( #14815, #25711, #6036, #1162, #23567, #14252, #16542, #3878 ),
 .UNSPECIFIED., .F., .F.,
 ( 4, 2, 2, 4 ),
 ( 0.03156115556267154870, 0.03330631506936942987, 0.03505147457606731104, 0.03854179358946310113 ),
 .UNSPECIFIED. ) ;
#15810 = DIRECTION ( 'NONE',  ( 1.000000000000000000, -0.000000000000000000, -0.000000000000000000 ) ) ;
#15812 = CARTESIAN_POINT ( 'NONE',  ( 90.17595424772805757, 111.7661400908348384, 72.22656249985354293 ) ) ;
#15813 = LINE ( 'NONE', #4865, #16468 ) ;
#15814 = FACE_OUTER_BOUND ( 'NONE', #6086, .T. ) ;
#15815 = DIRECTION ( 'NONE',  ( 0.000000000000000000, -1.000000000000000000, 0.000000000000000000 ) ) ;
#15816 = CARTESIAN_POINT ( 'NONE',  ( -68.97958094182604327, 102.2323340340523288, -145.0000000000000000 ) ) ;
#15818 = ORIENTED_EDGE ( 'NONE', *, *, #25209, .T. ) ;
#15817 = EDGE_LOOP ( 'NONE', ( #9566, #10868, #827, #23146 ) ) ;
#15819 = AXIS2_PLACEMENT_3D ( 'NONE', #22750, #14412, #7528 ) ;
#15820 = CARTESIAN_POINT ( 'NONE',  ( -208.7912193213397245, 88.73557081762633914, -26.19220075538009240 ) ) ;
#15821 = DIRECTION ( 'NONE',  ( -0.000000000000000000, -1.000000000000000000, -0.000000000000000000 ) ) ;
#15822 = CARTESIAN_POINT ( 'NONE',  ( -209.0043318837038555, 89.43882380443007207, -25.53063627850903217 ) ) ;
#15823 = ORIENTED_EDGE ( 'NONE', *, *, #27781, .T. ) ;
#15824 = VECTOR ( 'NONE', #10751, 1000.000000000000000 ) ;
#15825 = ORIENTED_EDGE ( 'NONE', *, *, #23518, .F. ) ;
#15826 = ORIENTED_EDGE ( 'NONE', *, *, #19536, .T. ) ;
#15827 = EDGE_CURVE ( 'NONE', #16038, #17953, #9927, .T. ) ;
#15828 = LINE ( 'NONE', #2871, #24415 ) ;
#15829 = CARTESIAN_POINT ( 'NONE',  ( -127.4298061085324889, 130.3533807148441213, 16.56307014168300995 ) ) ;
#15830 = VERTEX_POINT ( 'NONE', #10069 ) ;
#15831 = ORIENTED_EDGE ( 'NONE', *, *, #11177, .F. ) ;
#15832 = DIRECTION ( 'NONE',  ( -3.469446951953614189E-16, 1.000000000000000000, 0.000000000000000000 ) ) ;
#15833 = EDGE_CURVE ( 'NONE', #26033, #25738, #21258, .T. ) ;
#15834 = LINE ( 'NONE', #7201, #4073 ) ;
#15835 = EDGE_LOOP ( 'NONE', ( #23828, #10158, #2978, #13526 ) ) ;
#15836 = DIRECTION ( 'NONE',  ( 0.7071067811865475727, 0.7071067811865475727, -0.000000000000000000 ) ) ;
#15837 = AXIS2_PLACEMENT_3D ( 'NONE', #24406, #17367, #11347 ) ;
#15838 = CARTESIAN_POINT ( 'NONE',  ( 105.5625601981895585, 242.0882937662017014, -29.27845391395231545 ) ) ;
#15839 = EDGE_CURVE ( 'NONE', #13234, #24608, #23279, .T. ) ;
#15840 = LINE ( 'NONE', #15266, #28163 ) ;
#15841 = VECTOR ( 'NONE', #22938, 1000.000000000000114 ) ;
#15842 = DIRECTION ( 'NONE',  ( 1.000000000000000000, 0.000000000000000000, 0.000000000000000000 ) ) ;
#15843 = CARTESIAN_POINT ( 'NONE',  ( -195.1986077931981356, 62.83738171803135231, -37.97438512083786577 ) ) ;
#15844 = ORIENTED_EDGE ( 'NONE', *, *, #26911, .T. ) ;
#15845 = CARTESIAN_POINT ( 'NONE',  ( -12.24491960465745599, -18.01420295945611727, 80.00000000000001421 ) ) ;
#15846 = CARTESIAN_POINT ( 'NONE',  ( -219.9212092885467484, 137.1730549828544667, -15.11921763784017436 ) ) ;
#15847 = CARTESIAN_POINT ( 'NONE',  ( 157.4999999999997158, 261.3799376238655441, -45.00000000000000000 ) ) ;
#15848 = DIRECTION ( 'NONE',  ( 0.000000000000000000, 0.000000000000000000, 1.000000000000000000 ) ) ;
#15849 = ORIENTED_EDGE ( 'NONE', *, *, #24397, .F. ) ;
#15850 = DIRECTION ( 'NONE',  ( -0.000000000000000000, -0.000000000000000000, 1.000000000000000000 ) ) ;
#15851 = CARTESIAN_POINT ( 'NONE',  ( 79.99999999999991473, 139.9999999999999716, -45.00000000000000000 ) ) ;
#15852 = DIRECTION ( 'NONE',  ( 0.000000000000000000, 0.000000000000000000, -1.000000000000000000 ) ) ;
#15853 = ORIENTED_EDGE ( 'NONE', *, *, #5786, .F. ) ;
#15854 = VECTOR ( 'NONE', #3086, 1000.000000000000227 ) ;
#15855 = ORIENTED_EDGE ( 'NONE', *, *, #27561, .F. ) ;
#15856 = AXIS2_PLACEMENT_3D ( 'NONE', #4402, #26094, #1963 ) ;
#15857 = EDGE_CURVE ( 'NONE', #23432, #2973, #4726, .T. ) ;
#15858 = CARTESIAN_POINT ( 'NONE',  ( 94.38583646782731762, 113.6320904521816857, 75.15625000028097702 ) ) ;
#15859 = CARTESIAN_POINT ( 'NONE',  ( -201.5824907507999342, 94.41641349969115993, -29.50224322716549707 ) ) ;
#15860 = ORIENTED_EDGE ( 'NONE', *, *, #24459, .F. ) ;
#15861 = VECTOR ( 'NONE', #24455, 1000.000000000000000 ) ;
#15862 = ORIENTED_EDGE ( 'NONE', *, *, #2804, .F. ) ;
#15863 = CARTESIAN_POINT ( 'NONE',  ( 158.0000000000000284, 205.9527499549551806, 45.00000000000000000 ) ) ;
#15864 = LINE ( 'NONE', #7518, #27611 ) ;
#15865 = ORIENTED_EDGE ( 'NONE', *, *, #15371, .F. ) ;
#15866 = CARTESIAN_POINT ( 'NONE',  ( 91.70829090827390928, 81.72138244997330503, 100.0000000000000142 ) ) ;
#15867 = ORIENTED_EDGE ( 'NONE', *, *, #18052, .F. ) ;
#15868 = FACE_BOUND ( 'NONE', #17120, .T. ) ;
#15869 = EDGE_CURVE ( 'NONE', #2371, #14116, #24136, .T. ) ;
#15870 = EDGE_CURVE ( 'NONE', #19273, #17375, #21950, .T. ) ;
#15871 = DIRECTION ( 'NONE',  ( 0.8916010070293384215, 0.4528218681383106015, 0.000000000000000000 ) ) ;
#15872 = DIRECTION ( 'NONE',  ( -0.000000000000000000, 0.000000000000000000, -1.000000000000000000 ) ) ;
#15873 = CARTESIAN_POINT ( 'NONE',  ( -17.81748447342208053, 128.7387662681335883, -17.18977265686632094 ) ) ;
#15874 = CARTESIAN_POINT ( 'NONE',  ( 157.4999999999995168, 208.7145624662163925, -45.00000000000000000 ) ) ;
#15875 = AXIS2_PLACEMENT_3D ( 'NONE', #10084, #18836, #5764 ) ;
#15876 = LINE ( 'NONE', #776, #13813 ) ;
#15877 = FACE_OUTER_BOUND ( 'NONE', #6615, .T. ) ;
#15878 = VERTEX_POINT ( 'NONE', #15236 ) ;
#15879 = FACE_OUTER_BOUND ( 'NONE', #14257, .T. ) ;
#15880 = CIRCLE ( 'NONE', #3464, 9.999999999999998224 ) ;
#15881 = CARTESIAN_POINT ( 'NONE',  ( 193.7634559672933676, 193.7634559672857790, 45.00000000000000000 ) ) ;
#15882 = DIRECTION ( 'NONE',  ( -0.5975062131282562472, 0.8018642810807392607, 0.000000000000000000 ) ) ;
#15883 = LINE ( 'NONE', #11425, #3369 ) ;
#15884 = ORIENTED_EDGE ( 'NONE', *, *, #11274, .T. ) ;
#15885 = EDGE_CURVE ( 'NONE', #9167, #25901, #10777, .T. ) ;
#15886 = CARTESIAN_POINT ( 'NONE',  ( 158.0000000000011653, 93.60624962464788723, 45.00000000000000000 ) ) ;
#15887 = EDGE_LOOP ( 'NONE', ( #11823, #16586, #6514 ) ) ;
#15888 = EDGE_CURVE ( 'NONE', #11099, #15738, #23992, .T. ) ;
#15889 = LINE ( 'NONE', #26480, #11170 ) ;
#15890 = CARTESIAN_POINT ( 'NONE',  ( -248.1546605714623013, -91.18033988749901653, 0.000000000000000000 ) ) ;
#15891 = CARTESIAN_POINT ( 'NONE',  ( -189.5231184314577320, 157.6231267382823376, -13.00000000000000000 ) ) ;
#15892 = ORIENTED_EDGE ( 'NONE', *, *, #28296, .F. ) ;
#15893 = FACE_OUTER_BOUND ( 'NONE', #16938, .T. ) ;
#15894 = ORIENTED_EDGE ( 'NONE', *, *, #16693, .F. ) ;
#15895 = CARTESIAN_POINT ( 'NONE',  ( 157.4751130497509450, 224.9869122110685566, 45.00000000000000000 ) ) ;
#15896 = VERTEX_POINT ( 'NONE', #15382 ) ;
#15897 = CARTESIAN_POINT ( 'NONE',  ( -277.2150368962633706, -170.0000000000001137, -101.5769467933888137 ) ) ;
#15898 = EDGE_LOOP ( 'NONE', ( #19962, #5126, #9413, #5019 ) ) ;
#15899 = AXIS2_PLACEMENT_3D ( 'NONE', #11345, #20090, #22394 ) ;
#15900 = ADVANCED_FACE ( 'NONE', ( #17659 ), #19537, .F. ) ;
#15901 = VECTOR ( 'NONE', #20042, 1000.000000000000000 ) ;
#15902 = EDGE_LOOP ( 'NONE', ( #3186, #1949, #6333, #941 ) ) ;
#15903 = CARTESIAN_POINT ( 'NONE',  ( 157.4999999999998579, 50.71843699327460797, 45.00000000000000000 ) ) ;
#15904 = ORIENTED_EDGE ( 'NONE', *, *, #15508, .T. ) ;
#15905 = EDGE_LOOP ( 'NONE', ( #10898, #3784, #3852, #11613 ) ) ;
#15906 = AXIS2_PLACEMENT_3D ( 'NONE', #3479, #16707, #5496 ) ;
#15907 = ORIENTED_EDGE ( 'NONE', *, *, #14741, .T. ) ;
#15908 = CARTESIAN_POINT ( 'NONE',  ( 98.38958437018622760, 241.8303606468397220, 11.96405203492901137 ) ) ;
#15909 = CARTESIAN_POINT ( 'NONE',  ( -217.7401460507884110, 138.5677444271666161, 12.99353264133693742 ) ) ;
#15910 = FACE_OUTER_BOUND ( 'NONE', #21936, .T. ) ;
#15911 = CARTESIAN_POINT ( 'NONE',  ( 79.99999999999992895, 110.0000000000000000, -70.00000000000001421 ) ) ;
#15912 = DIRECTION ( 'NONE',  ( 0.000000000000000000, 0.000000000000000000, -1.000000000000000000 ) ) ;
#15913 = CARTESIAN_POINT ( 'NONE',  ( 179.9999999999999147, 494.4107529906318632, -84.99999999999997158 ) ) ;
#15914 = PLANE ( 'NONE',  #8568 ) ;
#15915 = DIRECTION ( 'NONE',  ( -0.8916010070298056034, -0.4528218681373908372, 0.000000000000000000 ) ) ;
#15916 = DIRECTION ( 'NONE',  ( 1.000000000000000000, 0.000000000000000000, 0.000000000000000000 ) ) ;
#15917 = FACE_OUTER_BOUND ( 'NONE', #27833, .T. ) ;
#15918 = CARTESIAN_POINT ( 'NONE',  ( 157.9999999999997442, 251.0945000900840398, 45.00000000000000000 ) ) ;
#15919 = TOROIDAL_SURFACE ( 'NONE', #3503, 55.86582179324592090, 2.000000000000000000 ) ;
#15920 = EDGE_LOOP ( 'NONE', ( #21694, #18504, #26422, #6551 ) ) ;
#15921 = CARTESIAN_POINT ( 'NONE',  ( 157.9999999999998863, 218.4921249924925348, 45.00000000000000000 ) ) ;
#15922 = DIRECTION ( 'NONE',  ( 0.8916010070298155954, 0.4528218681373709087, 0.000000000000000000 ) ) ;
#15923 = DIRECTION ( 'NONE',  ( -0.000000000000000000, -0.000000000000000000, -1.000000000000000000 ) ) ;
#15924 = DIRECTION ( 'NONE',  ( -0.3897722486529259234, 0.9209112846414913012, 1.118268497331688440E-16 ) ) ;
#15925 = VECTOR ( 'NONE', #9149, 1000.000000000000000 ) ;
#15926 = ORIENTED_EDGE ( 'NONE', *, *, #2928, .T. ) ;
#15927 = EDGE_CURVE ( 'NONE', #8811, #24580, #13224, .T. ) ;
#15928 = DIRECTION ( 'NONE',  ( 0.000000000000000000, 0.000000000000000000, 1.000000000000000000 ) ) ;
#15929 = ORIENTED_EDGE ( 'NONE', *, *, #22171, .F. ) ;
#15930 = DIRECTION ( 'NONE',  ( 0.4528218681381900867, -0.8916010070293997058, 0.000000000000000000 ) ) ;
#15931 = ORIENTED_EDGE ( 'NONE', *, *, #21007, .F. ) ;
#15932 = ORIENTED_EDGE ( 'NONE', *, *, #9877, .F. ) ;
#15933 = EDGE_LOOP ( 'NONE', ( #14967, #19697, #10111, #2869 ) ) ;
#15934 = ORIENTED_EDGE ( 'NONE', *, *, #19903, .F. ) ;
#15935 = CARTESIAN_POINT ( 'NONE',  ( 65.00000000000000000, -170.0000000000000853, -69.99999999999998579 ) ) ;
#15936 = AXIS2_PLACEMENT_3D ( 'NONE', #13272, #12853, #4350 ) ;
#15937 = DIRECTION ( 'NONE',  ( 0.000000000000000000, 0.000000000000000000, -1.000000000000000000 ) ) ;
#15938 = CARTESIAN_POINT ( 'NONE',  ( 109.9999999999999574, -120.0000000000000426, 70.00000000000001421 ) ) ;
#15939 = LINE ( 'NONE', #20655, #20636 ) ;
#15940 = DIRECTION ( 'NONE',  ( -1.000000000000000000, -0.000000000000000000, -0.000000000000000000 ) ) ;
#15941 = CARTESIAN_POINT ( 'NONE',  ( -224.2911920753103345, 72.03214051460449241, 18.76861173149748652 ) ) ;
#15942 = CARTESIAN_POINT ( 'NONE',  ( -295.0000000000001137, -157.0000000000000284, 60.00000000000002842 ) ) ;
#15943 = DIRECTION ( 'NONE',  ( -0.2066290158914389774, 0.9784193629480844034, 0.000000000000000000 ) ) ;
#15944 = ADVANCED_FACE ( 'NONE', ( #6736 ), #17093, .T. ) ;
#15945 = CARTESIAN_POINT ( 'NONE',  ( 79.99999999999995737, 98.29969375664606446, -93.85322876744665166 ) ) ;
#15946 = CARTESIAN_POINT ( 'NONE',  ( -210.6525827442121113, 88.81591185141229516, -22.91848360207728419 ) ) ;
#15947 = LINE ( 'NONE', #13502, #15197 ) ;
#15948 = CARTESIAN_POINT ( 'NONE',  ( 85.90765579575223398, 110.5723347142863702, 70.58593750014345858 ) ) ;
#15949 = CARTESIAN_POINT ( 'NONE',  ( -11.46153413423660794, 131.5065341654955091, 16.18491763777246462 ) ) ;
#15950 = LINE ( 'NONE', #2569, #10994 ) ;
#15951 = CARTESIAN_POINT ( 'NONE',  ( -178.7338692018542474, 110.4480143559095069, 30.37507499509654352 ) ) ;
#15952 = ADVANCED_FACE ( 'NONE', ( #8621 ), #17371, .F. ) ;
#15953 = CARTESIAN_POINT ( 'NONE',  ( 25.90578987075423001, -14.95671475544977724, 45.00000000000000000 ) ) ;
#15955 = ORIENTED_EDGE ( 'NONE', *, *, #27982, .T. ) ;
#15954 = VERTEX_POINT ( 'NONE', #6602 ) ;
#15956 = VECTOR ( 'NONE', #27284, 1000.000000000000000 ) ;
#15957 = DIRECTION ( 'NONE',  ( 1.000000000000000000, -0.000000000000000000, -0.000000000000000000 ) ) ;
#15958 = ADVANCED_FACE ( 'NONE', ( #13086 ), #7173, .T. ) ;
#15960 = EDGE_CURVE ( 'NONE', #27632, #24388, #13505, .T. ) ;
#15959 = VECTOR ( 'NONE', #16219, 1000.000000000000114 ) ;
#15961 = CARTESIAN_POINT ( 'NONE',  ( 157.4999999999996874, 266.3956876388795649, 45.00000000000000000 ) ) ;
#15962 = EDGE_CURVE ( 'NONE', #10433, #13314, #289, .T. ) ;
#15963 = ORIENTED_EDGE ( 'NONE', *, *, #14232, .T. ) ;
#15964 = ORIENTED_EDGE ( 'NONE', *, *, #18117, .F. ) ;
#15965 = EDGE_LOOP ( 'NONE', ( #20608, #11299, #19616, #3534 ) ) ;
#15966 = DIRECTION ( 'NONE',  ( -0.000000000000000000, -0.000000000000000000, -1.000000000000000000 ) ) ;
#15967 = CARTESIAN_POINT ( 'NONE',  ( -151.1419734269974242, 123.3149796224834063, 20.04527379734153314 ) ) ;
#15968 = VERTEX_POINT ( 'NONE', #17948 ) ;
#15969 = VERTEX_POINT ( 'NONE', #26699 ) ;
#15970 = DIRECTION ( 'NONE',  ( -1.000000000000000000, 0.000000000000000000, 0.000000000000000000 ) ) ;
#15971 = LINE ( 'NONE', #27149, #3073 ) ;
#15972 = AXIS2_PLACEMENT_3D ( 'NONE', #28021, #16709, #1469 ) ;
#15973 = DIRECTION ( 'NONE',  ( 0.000000000000000000, 0.000000000000000000, -1.000000000000000000 ) ) ;
#15974 = ORIENTED_EDGE ( 'NONE', *, *, #19922, .F. ) ;
#15975 = DIRECTION ( 'NONE',  ( 1.000000000000000000, 0.000000000000000000, 0.000000000000000000 ) ) ;
#15976 = VECTOR ( 'NONE', #27524, 1000.000000000000000 ) ;
#15977 = DIRECTION ( 'NONE',  ( 0.4528218681376912080, 0.8916010070296530587, -0.000000000000000000 ) ) ;
#15978 = TOROIDAL_SURFACE ( 'NONE', #7251, 21.49999999999998224, 1.000000000000000000 ) ;
#15979 = LINE ( 'NONE', #5460, #22255 ) ;
#15980 = LINE ( 'NONE', #24871, #14585 ) ;
#15981 = CARTESIAN_POINT ( 'NONE',  ( -213.3516035875686896, 56.48049070729078380, -40.70111258791201436 ) ) ;
#15982 = EDGE_CURVE ( 'NONE', #2906, #24382, #15813, .T. ) ;
#15983 = EDGE_CURVE ( 'NONE', #24382, #26112, #22402, .T. ) ;
#15984 = DIRECTION ( 'NONE',  ( 1.000000000000000000, 0.000000000000000000, 0.000000000000000000 ) ) ;
#15985 = LINE ( 'NONE', #2744, #23907 ) ;
#15986 = CARTESIAN_POINT ( 'NONE',  ( 158.0000000000001990, 186.3976249024084666, -45.00000000000000000 ) ) ;
#15987 = DIRECTION ( 'NONE',  ( -0.000000000000000000, -0.000000000000000000, 1.000000000000000000 ) ) ;
#15988 = ORIENTED_EDGE ( 'NONE', *, *, #3596, .T. ) ;
#15989 = DIRECTION ( 'NONE',  ( -0.9209112846414913012, -0.3897722486529259789, 0.000000000000000000 ) ) ;
#15990 = AXIS2_PLACEMENT_3D ( 'NONE', #11350, #22400, #22253 ) ;
#15991 = ADVANCED_FACE ( 'NONE', ( #20242 ), #22427, .F. ) ;
#15992 = DIRECTION ( 'NONE',  ( 1.000000000000000000, 0.000000000000000000, 0.000000000000000000 ) ) ;
#15993 = AXIS2_PLACEMENT_3D ( 'NONE', #21724, #6767, #13254 ) ;
#15994 = LINE ( 'NONE', #22010, #15405 ) ;
#15995 = ORIENTED_EDGE ( 'NONE', *, *, #8181, .T. ) ;
#15996 = ORIENTED_EDGE ( 'NONE', *, *, #20287, .T. ) ;
#15997 = DIRECTION ( 'NONE',  ( -0.000000000000000000, -0.000000000000000000, -1.000000000000000000 ) ) ;
#15998 = DIRECTION ( 'NONE',  ( -0.000000000000000000, 0.000000000000000000, -1.000000000000000000 ) ) ;
#15999 = VERTEX_POINT ( 'NONE', #7987 ) ;
#16000 = ORIENTED_EDGE ( 'NONE', *, *, #25785, .T. ) ;
#16001 = PLANE ( 'NONE',  #10424 ) ;
#16002 = DIRECTION ( 'NONE',  ( 0.8916010070297142320, 0.4528218681375707488, 0.000000000000000000 ) ) ;
#16003 = CIRCLE ( 'NONE', #3582, 16.46313063346208239 ) ;
#16004 = ORIENTED_EDGE ( 'NONE', *, *, #9025, .F. ) ;
#16005 = FACE_OUTER_BOUND ( 'NONE', #4200, .T. ) ;
#16006 = ORIENTED_EDGE ( 'NONE', *, *, #22794, .F. ) ;
#16007 = PLANE ( 'NONE',  #14373 ) ;
#16008 = AXIS2_PLACEMENT_3D ( 'NONE', #24808, #9152, #17910 ) ;
#16009 = AXIS2_PLACEMENT_3D ( 'NONE', #7732, #3124, #25531 ) ;
#16010 = DIRECTION ( 'NONE',  ( -0.000000000000000000, -0.000000000000000000, -1.000000000000000000 ) ) ;
#16011 = LINE ( 'NONE', #5495, #17168 ) ;
#16012 = CARTESIAN_POINT ( 'NONE',  ( 9.345921402568846403, 139.9999999999999716, -15.00000000000000000 ) ) ;
#16013 = CARTESIAN_POINT ( 'NONE',  ( 232.4999999999996305, 83.06687458711267880, -42.86484227207692754 ) ) ;
#16014 = CARTESIAN_POINT ( 'NONE',  ( -266.3253780546114626, -165.6690032019043599, -89.33268690869475392 ) ) ;
#16015 = CARTESIAN_POINT ( 'NONE',  ( 157.4999999999998010, 241.3169375638095460, 45.00000000000000000 ) ) ;
#16016 = EDGE_CURVE ( 'NONE', #12285, #13130, #25507, .T. ) ;
#16017 = ORIENTED_EDGE ( 'NONE', *, *, #17067, .F. ) ;
#16018 = DIRECTION ( 'NONE',  ( 0.000000000000000000, -1.000000000000000000, 0.000000000000000000 ) ) ;
#16019 = FACE_OUTER_BOUND ( 'NONE', #1033, .T. ) ;
#16020 = DIRECTION ( 'NONE',  ( 0.000000000000000000, 0.000000000000000000, 1.000000000000000000 ) ) ;
#16021 = CARTESIAN_POINT ( 'NONE',  ( 158.0000000000010232, 108.1456246621830957, -45.00000000000000000 ) ) ;
#16022 = ORIENTED_EDGE ( 'NONE', *, *, #2989, .T. ) ;
#16023 = CARTESIAN_POINT ( 'NONE',  ( 123.9999999999998579, 220.0000000000000284, 99.00000000000001421 ) ) ;
#16024 = ORIENTED_EDGE ( 'NONE', *, *, #25437, .F. ) ;
#16025 = AXIS2_PLACEMENT_3D ( 'NONE', #11536, #461, #18130 ) ;
#16026 = DIRECTION ( 'NONE',  ( -0.000000000000000000, -0.000000000000000000, -1.000000000000000000 ) ) ;
#16027 = CARTESIAN_POINT ( 'NONE',  ( 157.4999999999997158, 258.8720626163585621, -45.00000000000000000 ) ) ;
#16028 = CARTESIAN_POINT ( 'NONE',  ( 9.999999999999957367, -20.00000000000004974, 100.0000000000000142 ) ) ;
#16029 = EDGE_LOOP ( 'NONE', ( #25906, #9911, #7146, #6722, #26713 ) ) ;
#16030 = DIRECTION ( 'NONE',  ( 0.000000000000000000, 0.000000000000000000, 1.000000000000000000 ) ) ;
#16031 = EDGE_LOOP ( 'NONE', ( #25976, #2058, #9935, #11356 ) ) ;
#16032 = EDGE_CURVE ( 'NONE', #21598, #695, #10287, .T. ) ;
#16033 = DIRECTION ( 'NONE',  ( 0.000000000000000000, 0.000000000000000000, 1.000000000000000000 ) ) ;
#16034 = ORIENTED_EDGE ( 'NONE', *, *, #10567, .F. ) ;
#16035 = ADVANCED_FACE ( 'NONE', ( #8127 ), #14598, .F. ) ;
#16036 = CARTESIAN_POINT ( 'NONE',  ( 157.9999999999996589, 276.6811251726610976, 45.00000000000000000 ) ) ;
#16037 = ORIENTED_EDGE ( 'NONE', *, *, #24060, .T. ) ;
#16038 = VERTEX_POINT ( 'NONE', #28069 ) ;
#16039 = CARTESIAN_POINT ( 'NONE',  ( 157.9999999999996589, 279.1890001801680796, 45.00000000000000000 ) ) ;
#16040 = ORIENTED_EDGE ( 'NONE', *, *, #16628, .T. ) ;
#16041 = ORIENTED_EDGE ( 'NONE', *, *, #18403, .F. ) ;
#16042 = ORIENTED_EDGE ( 'NONE', *, *, #9265, .T. ) ;
#16043 = ADVANCED_FACE ( 'NONE', ( #19466 ), #8412, .F. ) ;
#16044 = CARTESIAN_POINT ( 'NONE',  ( 107.0062495987318272, 249.1467455478686759, 31.68887795644912586 ) ) ;
#16045 = EDGE_CURVE ( 'NONE', #6225, #10678, #3948, .T. ) ;
#16046 = VECTOR ( 'NONE', #14855, 1000.000000000000000 ) ;
#16047 = CARTESIAN_POINT ( 'NONE',  ( 157.9999999999998295, 224.0157500150140208, 45.00000000000000000 ) ) ;
#16048 = VECTOR ( 'NONE', #26226, 1000.000000000000000 ) ;
#16049 = CARTESIAN_POINT ( 'NONE',  ( -223.3099978423094001, 137.4510275522738993, -14.96944044186858491 ) ) ;
#16050 = CARTESIAN_POINT ( 'NONE',  ( 158.0000000000015348, 58.49599951954928656, 45.00000000000000000 ) ) ;
#16051 = CIRCLE ( 'NONE', #17401, 5.000000000000004441 ) ;
#16052 = DIRECTION ( 'NONE',  ( -0.000000000000000000, 1.000000000000000000, -1.387778780781445429E-16 ) ) ;
#16053 = CARTESIAN_POINT ( 'NONE',  ( 93.99999999999985789, 171.5103103742661972, -84.99999999999997158 ) ) ;
#16054 = CARTESIAN_POINT ( 'NONE',  ( -233.2943309833551950, 92.06151970357237246, -13.00000000000000000 ) ) ;
#16055 = DIRECTION ( 'NONE',  ( -1.000000000000000000, -0.000000000000000000, -0.000000000000000000 ) ) ;
#16056 = CARTESIAN_POINT ( 'NONE',  ( 144.9999999999998863, 220.0000000000000284, 90.00000000000002842 ) ) ;
#16057 = CARTESIAN_POINT ( 'NONE',  ( 158.0000000000017053, 43.44874947450702507, 45.00000000000000000 ) ) ;
#16058 = DIRECTION ( 'NONE',  ( 0.9784193629480781862, -0.2066290158914688702, 0.000000000000000000 ) ) ;
#16059 = VERTEX_POINT ( 'NONE', #23354 ) ;
#16060 = DIRECTION ( 'NONE',  ( -1.000000000000000000, 0.000000000000000000, 0.000000000000000000 ) ) ;
#16061 = AXIS2_PLACEMENT_3D ( 'NONE', #19237, #10622, #8037 ) ;
#16062 = DIRECTION ( 'NONE',  ( 1.000000000000000000, 0.000000000000000000, 0.000000000000000000 ) ) ;
#16063 = DIRECTION ( 'NONE',  ( 1.000000000000000000, -0.000000000000000000, -0.000000000000000000 ) ) ;
#16064 = DIRECTION ( 'NONE',  ( -0.000000000000000000, -0.000000000000000000, -1.000000000000000000 ) ) ;
#16065 = EDGE_LOOP ( 'NONE', ( #27721, #20754, #10245, #14974 ) ) ;
#16066 = EDGE_CURVE ( 'NONE', #15103, #27621, #10147, .T. ) ;
#16067 = ADVANCED_FACE ( 'NONE', ( #27648 ), #12736, .T. ) ;
#16068 = AXIS2_PLACEMENT_3D ( 'NONE', #26860, #15957, #24709 ) ;
#16069 = DIRECTION ( 'NONE',  ( -0.000000000000000000, -0.000000000000000000, -1.000000000000000000 ) ) ;
#16070 = ORIENTED_EDGE ( 'NONE', *, *, #26101, .F. ) ;
#16071 = SURFACE_STYLE_FILL_AREA ( #5276 ) ;
#16072 = AXIS2_PLACEMENT_3D ( 'NONE', #11780, #11195, #13498 ) ;
#16073 = ORIENTED_EDGE ( 'NONE', *, *, #549, .F. ) ;
#16074 = VECTOR ( 'NONE', #20637, 1000.000000000000000 ) ;
#16075 = ORIENTED_EDGE ( 'NONE', *, *, #21468, .F. ) ;
#16076 = ORIENTED_EDGE ( 'NONE', *, *, #25247, .T. ) ;
#16077 = ORIENTED_EDGE ( 'NONE', *, *, #10519, .F. ) ;
#16078 = DIRECTION ( 'NONE',  ( -0.7071067811865336949, 0.7071067811865613395, 0.000000000000000000 ) ) ;
#16079 = EDGE_CURVE ( 'NONE', #9426, #10893, #1317, .T. ) ;
#16080 = CARTESIAN_POINT ( 'NONE',  ( 157.4999999999998579, 183.6358123911478799, 45.00000000000000000 ) ) ;
#16081 = DIRECTION ( 'NONE',  ( -1.000000000000000000, -0.000000000000000000, -0.000000000000000000 ) ) ;
#16082 = CARTESIAN_POINT ( 'NONE',  ( -107.7681813716040580, 133.6595412580404059, -15.67431181523478578 ) ) ;
#16083 = EDGE_CURVE ( 'NONE', #5476, #13728, #16755, .T. ) ;
#16084 = DIRECTION ( 'NONE',  ( -0.000000000000000000, 1.000000000000000000, -1.387778780781445429E-16 ) ) ;
#16085 = EDGE_CURVE ( 'NONE', #20337, #14862, #4090, .T. ) ;
#16086 = CARTESIAN_POINT ( 'NONE',  ( -213.7039558558103352, 55.82027786946292025, 42.47917487896670963 ) ) ;
#16087 = DIRECTION ( 'NONE',  ( 0.000000000000000000, -1.000000000000000000, 0.000000000000000000 ) ) ;
#16088 = DIRECTION ( 'NONE',  ( 1.000000000000000000, 0.000000000000000000, -1.224646799147353207E-16 ) ) ;
#16089 = AXIS2_PLACEMENT_3D ( 'NONE', #9286, #3231, #13753 ) ;
#16090 = CARTESIAN_POINT ( 'NONE',  ( 79.99999999999995737, 106.0349479707060993, -85.03452022453005554 ) ) ;
#16091 = CARTESIAN_POINT ( 'NONE',  ( -204.2442923823817011, 92.17690269152525673, -28.15093001741121981 ) ) ;
#16092 = EDGE_CURVE ( 'NONE', #3858, #1788, #5744, .T. ) ;
#16093 = DIRECTION ( 'NONE',  ( 0.000000000000000000, 0.000000000000000000, -1.000000000000000000 ) ) ;
#16094 = LINE ( 'NONE', #2419, #16212 ) ;
#16095 = VECTOR ( 'NONE', #4430, 1000.000000000000000 ) ;
#16096 = CARTESIAN_POINT ( 'NONE',  ( 65.00000000000000000, -170.0000000000000853, -64.00000000000001421 ) ) ;
#16097 = CARTESIAN_POINT ( 'NONE',  ( 91.70829090828171104, 81.72138244998292578, -100.0000000000000284 ) ) ;
#16098 = LINE ( 'NONE', #11355, #25356 ) ;
#16100 = EDGE_LOOP ( 'NONE', ( #19521, #7913, #25341, #5975 ) ) ;
#16099 = ORIENTED_EDGE ( 'NONE', *, *, #885, .F. ) ;
#16101 = CARTESIAN_POINT ( 'NONE',  ( -203.8025521703607694, 92.07732029363670279, -29.54281560658175465 ) ) ;
#16102 = DIRECTION ( 'NONE',  ( 1.000000000000000000, 0.000000000000000000, 0.000000000000000000 ) ) ;
#16103 = ORIENTED_EDGE ( 'NONE', *, *, #27328, .F. ) ;
#16104 = EDGE_CURVE ( 'NONE', #22985, #15009, #10712, .T. ) ;
#16105 = EDGE_LOOP ( 'NONE', ( #17024, #24465, #19089, #25338 ) ) ;
#16106 = DIRECTION ( 'NONE',  ( -1.000000000000000000, -3.469446951953614189E-16, 0.000000000000000000 ) ) ;
#16107 = VECTOR ( 'NONE', #20626, 1000.000000000000114 ) ;
#16108 = CARTESIAN_POINT ( 'NONE',  ( -127.8937336576301220, 131.6565518472861243, 14.66727481766007202 ) ) ;
#16109 = EDGE_LOOP ( 'NONE', ( #519, #2257, #2355, #22878, #23318 ) ) ;
#16110 = EDGE_LOOP ( 'NONE', ( #22746, #13072, #26449 ) ) ;
#16111 = CARTESIAN_POINT ( 'NONE',  ( 157.4999999999998579, 183.6358123911478799, -45.00000000000000000 ) ) ;
#16112 = CARTESIAN_POINT ( 'NONE',  ( 157.4999999999997726, 243.8248125713165280, 45.00000000000000000 ) ) ;
#16113 = AXIS2_PLACEMENT_3D ( 'NONE', #2676, #21937, #11468 ) ;
#16114 = DIRECTION ( 'NONE',  ( -0.8916010070294706491, -0.4528218681380501986, 0.000000000000000000 ) ) ;
#16115 = CARTESIAN_POINT ( 'NONE',  ( -203.1779787704217028, 93.05164332230201296, 28.77272332722131054 ) ) ;
#16116 = CARTESIAN_POINT ( 'NONE',  ( 157.9999999999997442, 251.0945000900840398, -45.00000000000000000 ) ) ;
#16117 = ADVANCED_FACE ( 'NONE', ( #10566 ), #14740, .F. ) ;
#16118 = EDGE_CURVE ( 'NONE', #17857, #27076, #25167, .T. ) ;
#16119 = LINE ( 'NONE', #14380, #25007 ) ;
#16120 = CARTESIAN_POINT ( 'NONE',  ( 157.4999999999998579, 120.9389372034718093, 45.00000000000000000 ) ) ;
#16121 = CARTESIAN_POINT ( 'NONE',  ( -207.6173544636101553, 75.51556044650348554, -42.73482814336003344 ) ) ;
#16122 = AXIS2_PLACEMENT_3D ( 'NONE', #24024, #15810, #13797 ) ;
#16123 = CYLINDRICAL_SURFACE ( 'NONE', #28366, 10.00000000000000888 ) ;
#16124 = FACE_OUTER_BOUND ( 'NONE', #16864, .T. ) ;
#16125 = CARTESIAN_POINT ( 'NONE',  ( 158.0000000000006537, 145.7637497747887210, -45.00000000000000000 ) ) ;
#16126 = DIRECTION ( 'NONE',  ( 1.000000000000000000, 3.004539147878382249E-48, 2.775557561562887407E-16 ) ) ;
#16127 = ORIENTED_EDGE ( 'NONE', *, *, #24935, .T. ) ;
#16128 = LINE ( 'NONE', #26743, #24287 ) ;
#16129 = VECTOR ( 'NONE', #6459, 1000.000000000000000 ) ;
#16130 = CARTESIAN_POINT ( 'NONE',  ( -236.8177751472017007, 82.33896643611701904, 15.00000000000000000 ) ) ;
#16131 = CARTESIAN_POINT ( 'NONE',  ( 134.9999999999998579, 404.6636166603179277, -145.0000000000000000 ) ) ;
#16132 = ORIENTED_EDGE ( 'NONE', *, *, #20151, .T. ) ;
#16133 = ORIENTED_EDGE ( 'NONE', *, *, #17290, .F. ) ;
#16134 = CARTESIAN_POINT ( 'NONE',  ( 107.3061218088239883, 127.3934823310315920, 99.99999999997838529 ) ) ;
#16135 = CARTESIAN_POINT ( 'NONE',  ( 158.0000000000001990, 188.3976249024084666, 45.00000000000000000 ) ) ;
#16136 = EDGE_LOOP ( 'NONE', ( #18953, #623, #3932, #22042 ) ) ;
#16137 = EDGE_LOOP ( 'NONE', ( #766, #4978, #9346, #5865 ) ) ;
#16138 = CARTESIAN_POINT ( 'NONE',  ( -180.0000000000000284, -50.00000000000004263, 80.00000000000001421 ) ) ;
#16139 = CIRCLE ( 'NONE', #3723, 1.000000000000000888 ) ;
#16140 = CARTESIAN_POINT ( 'NONE',  ( 46.36636626309694975, -15.13258561588589757, 45.00000000000000000 ) ) ;
#16141 = DIRECTION ( 'NONE',  ( -0.000000000000000000, 0.000000000000000000, -1.000000000000000000 ) ) ;
#16142 = VERTEX_POINT ( 'NONE', #16615 ) ;
#16143 = DIRECTION ( 'NONE',  ( 0.000000000000000000, 0.000000000000000000, -1.000000000000000000 ) ) ;
#16144 = ORIENTED_EDGE ( 'NONE', *, *, #15329, .F. ) ;
#16145 = AXIS2_PLACEMENT_3D ( 'NONE', #1207, #16447, #27619 ) ;
#16146 = CARTESIAN_POINT ( 'NONE',  ( 157.4999999999998295, 226.2696875187675118, -45.00000000000000000 ) ) ;
#16147 = EDGE_CURVE ( 'NONE', #12751, #26586, #23216, .T. ) ;
#16148 = AXIS2_PLACEMENT_3D ( 'NONE', #4411, #7578, #13914 ) ;
#16149 = EDGE_CURVE ( 'NONE', #25123, #20874, #21051, .T. ) ;
#16150 = CARTESIAN_POINT ( 'NONE',  ( 158.0000000000001137, 195.9212499249295831, -45.00000000000000000 ) ) ;
#16151 = CARTESIAN_POINT ( 'NONE',  ( -175.0000000000000000, -170.0000000000001990, -69.99999999999998579 ) ) ;
#16152 = CARTESIAN_POINT ( 'NONE',  ( -6.744242412876251258, 131.5654230417238466, -16.20713396055394995 ) ) ;
#16153 = CARTESIAN_POINT ( 'NONE',  ( 65.00000000000000000, -120.0250000000000909, -76.00000000000000000 ) ) ;
#16154 = DIRECTION ( 'NONE',  ( -0.000000000000000000, -0.000000000000000000, -1.000000000000000000 ) ) ;
#16155 = DIRECTION ( 'NONE',  ( -0.000000000000000000, -0.000000000000000000, -1.000000000000000000 ) ) ;
#16156 = VERTEX_POINT ( 'NONE', #68 ) ;
#16157 = CARTESIAN_POINT ( 'NONE',  ( 1.982541115402066017E-14, -150.0000000000000568, 110.0000000000000284 ) ) ;
#16158 = CARTESIAN_POINT ( 'NONE',  ( -237.3870311360069536, 121.7710280244218950, 15.00000000000000000 ) ) ;
#16159 = CARTESIAN_POINT ( 'NONE',  ( 64.99999999999998579, -173.6051637141654282, 70.00000000000002842 ) ) ;
#16160 = DIRECTION ( 'NONE',  ( 0.000000000000000000, -0.000000000000000000, -1.000000000000000000 ) ) ;
#16161 = VERTEX_POINT ( 'NONE', #15453 ) ;
#16162 = DIRECTION ( 'NONE',  ( -0.8314772792026905446, 0.5555587585212667934, 0.000000000000000000 ) ) ;
#16163 = ORIENTED_EDGE ( 'NONE', *, *, #17685, .F. ) ;
#16164 = VECTOR ( 'NONE', #5505, 1000.000000000000000 ) ;
#16165 = CARTESIAN_POINT ( 'NONE',  ( 157.4999999999998010, 236.3011875487955251, 45.00000000000000000 ) ) ;
#16166 = CARTESIAN_POINT ( 'NONE',  ( -215.7935364303660322, 60.28281843632714754, -13.31033261678753910 ) ) ;
#16167 = DIRECTION ( 'NONE',  ( -1.000000000000000000, 0.000000000000000000, 0.000000000000000000 ) ) ;
#16168 = VERTEX_POINT ( 'NONE', #21768 ) ;
#16169 = CARTESIAN_POINT ( 'NONE',  ( -305.0000000000001137, -170.0000000000001137, 60.00000000000002842 ) ) ;
#16170 = DIRECTION ( 'NONE',  ( -0.000000000000000000, -0.000000000000000000, -1.000000000000000000 ) ) ;
#16171 = AXIS2_PLACEMENT_3D ( 'NONE', #25483, #23610, #5940 ) ;
#16172 = VERTEX_POINT ( 'NONE', #6391 ) ;
#16173 = AXIS2_PLACEMENT_3D ( 'NONE', #7507, #5338, #5475 ) ;
#16174 = AXIS2_PLACEMENT_3D ( 'NONE', #2941, #7112, #25066 ) ;
#16175 = PLANE ( 'NONE',  #13459 ) ;
#16176 = CARTESIAN_POINT ( 'NONE',  ( 158.0000000000001421, 193.4133749174225443, 45.00000000000000000 ) ) ;
#16177 = EDGE_LOOP ( 'NONE', ( #14834, #4247, #22055, #4943 ) ) ;
#16178 = EDGE_CURVE ( 'NONE', #27270, #3147, #2074, .T. ) ;
#16179 = ORIENTED_EDGE ( 'NONE', *, *, #28285, .F. ) ;
#16180 = DIRECTION ( 'NONE',  ( 0.000000000000000000, -1.000000000000000000, 0.000000000000000000 ) ) ;
#16181 = ORIENTED_EDGE ( 'NONE', *, *, #20355, .F. ) ;
#16182 = ADVANCED_FACE ( 'NONE', ( #15591 ), #2492, .F. ) ;
#16183 = ORIENTED_EDGE ( 'NONE', *, *, #12318, .F. ) ;
#16184 = ORIENTED_EDGE ( 'NONE', *, *, #25586, .T. ) ;
#16185 = TOROIDAL_SURFACE ( 'NONE', #3770, -538.1631314933625845, 562.1290781602207289 ) ;
#16186 = LINE ( 'NONE', #5105, #14799 ) ;
#16187 = AXIS2_PLACEMENT_3D ( 'NONE', #10493, #27996, #17097 ) ;
#16188 = EDGE_CURVE ( 'NONE', #9224, #21137, #4371, .T. ) ;
#16189 = DIRECTION ( 'NONE',  ( 0.8916010070293584056, 0.4528218681382713551, 0.000000000000000000 ) ) ;
#16190 = CARTESIAN_POINT ( 'NONE',  ( 157.9999999999996589, 273.6653751576470768, 45.00000000000000000 ) ) ;
#16191 = AXIS2_PLACEMENT_3D ( 'NONE', #13612, #246, #9004 ) ;
#16192 = AXIS2_PLACEMENT_3D ( 'NONE', #9973, #23747, #25610 ) ;
#16193 = DIRECTION ( 'NONE',  ( -0.000000000000000000, -0.000000000000000000, -1.000000000000000000 ) ) ;
#16194 = CARTESIAN_POINT ( 'NONE',  ( 158.0000000000013927, 73.54324956459154805, 45.00000000000000000 ) ) ;
#16195 = CARTESIAN_POINT ( 'NONE',  ( 121.6232796275294277, 239.4748271322486630, -45.00000000000000000 ) ) ;
#16196 = ADVANCED_FACE ( 'NONE', ( #24337 ), #23922, .F. ) ;
#16197 = LINE ( 'NONE', #16470, #27354 ) ;
#16198 = LINE ( 'NONE', #20631, #14474 ) ;
#16199 = DIRECTION ( 'NONE',  ( 1.000000000000000000, -0.000000000000000000, -0.000000000000000000 ) ) ;
#16200 = LINE ( 'NONE', #20350, #12338 ) ;
#16201 = CARTESIAN_POINT ( 'NONE',  ( 0.000000000000000000, 196.9999999999997442, 45.00000000000000000 ) ) ;
#16202 = EDGE_LOOP ( 'NONE', ( #26828, #25131, #7265, #26362 ) ) ;
#16203 = FACE_OUTER_BOUND ( 'NONE', #12382, .T. ) ;
#16204 = CARTESIAN_POINT ( 'NONE',  ( -180.0000000000000284, -40.00000000000004974, 110.0000000000000284 ) ) ;
#16205 = DIRECTION ( 'NONE',  ( 0.4999999999999881206, -0.8660254037844455910, 0.000000000000000000 ) ) ;
#16206 = ORIENTED_EDGE ( 'NONE', *, *, #9233, .T. ) ;
#16207 = EDGE_CURVE ( 'NONE', #14507, #553, #27473, .T. ) ;
#16208 = VECTOR ( 'NONE', #20619, 1000.000000000000000 ) ;
#16209 = AXIS2_PLACEMENT_3D ( 'NONE', #23116, #19324, #14891 ) ;
#16210 = PLANE ( 'NONE',  #4721 ) ;
#16211 = ORIENTED_EDGE ( 'NONE', *, *, #24532, .F. ) ;
#16212 = VECTOR ( 'NONE', #288, 1000.000000000000000 ) ;
#16213 = ORIENTED_EDGE ( 'NONE', *, *, #17927, .T. ) ;
#16214 = VECTOR ( 'NONE', #9126, 1000.000000000000000 ) ;
#16215 = ADVANCED_FACE ( 'NONE', ( #10851 ), #2208, .F. ) ;
#16216 = ORIENTED_EDGE ( 'NONE', *, *, #22717, .F. ) ;
#16217 = ORIENTED_EDGE ( 'NONE', *, *, #26940, .F. ) ;
#16218 = ORIENTED_EDGE ( 'NONE', *, *, #13137, .F. ) ;
#16219 = DIRECTION ( 'NONE',  ( 0.4528218681382910060, 0.8916010070293484135, 0.000000000000000000 ) ) ;
#16220 = DIRECTION ( 'NONE',  ( 0.4528218681374307497, -0.8916010070297853973, 0.000000000000000000 ) ) ;
#16221 = DIRECTION ( 'NONE',  ( 0.5000000000000039968, 0.8660254037844362651, 0.000000000000000000 ) ) ;
#16222 = CARTESIAN_POINT ( 'NONE',  ( -82.58612381453100681, 136.4858469420659333, -13.47871251474561305 ) ) ;
#16223 = DIRECTION ( 'NONE',  ( 0.000000000000000000, 0.000000000000000000, -1.000000000000000000 ) ) ;
#16224 = VECTOR ( 'NONE', #21321, 1000.000000000000000 ) ;
#16225 = CARTESIAN_POINT ( 'NONE',  ( -210.0090741174316804, 73.93180346605655018, 34.41452853221989727 ) ) ;
#16226 = CARTESIAN_POINT ( 'NONE',  ( -210.0000000000000568, -213.8933171992501059, 90.09368185681027796 ) ) ;
#16227 = DIRECTION ( 'NONE',  ( -0.000000000000000000, -0.000000000000000000, -1.000000000000000000 ) ) ;
#16228 = ADVANCED_FACE ( 'NONE', ( #15314 ), #2349, .F. ) ;
#16229 = EDGE_CURVE ( 'NONE', #1981, #7228, #17588, .T. ) ;
#16230 = CARTESIAN_POINT ( 'NONE',  ( 79.99999999999997158, 89.66646975086555926, -98.46778313769407021 ) ) ;
#16231 = DIRECTION ( 'NONE',  ( 0.000000000000000000, 0.000000000000000000, 1.000000000000000000 ) ) ;
#16232 = CIRCLE ( 'NONE', #21707, 20.00000000000001776 ) ;
#16233 = CARTESIAN_POINT ( 'NONE',  ( -212.2419371577844345, -220.0000000000000853, -110.0000000000000284 ) ) ;
#16234 = FACE_OUTER_BOUND ( 'NONE', #27350, .T. ) ;
#16235 = LINE ( 'NONE', #26697, #11153 ) ;
#16236 = CARTESIAN_POINT ( 'NONE',  ( 157.9999999999996874, 266.1417501351260171, 45.00000000000000000 ) ) ;
#16237 = FACE_OUTER_BOUND ( 'NONE', #1279, .T. ) ;
#16238 = CARTESIAN_POINT ( 'NONE',  ( -40.40953891503691153, 0.000000000000000000, 100.0000000000000000 ) ) ;
#16240 = ORIENTED_EDGE ( 'NONE', *, *, #18193, .F. ) ;
#16239 = ORIENTED_EDGE ( 'NONE', *, *, #16462, .T. ) ;
#16241 = EDGE_CURVE ( 'NONE', #22232, #17818, #26627, .T. ) ;
#16242 = DIRECTION ( 'NONE',  ( -0.8916010070295309342, 0.4528218681379315713, 0.000000000000000000 ) ) ;
#16243 = ORIENTED_EDGE ( 'NONE', *, *, #2678, .T. ) ;
#16244 = VECTOR ( 'NONE', #21994, 1000.000000000000000 ) ;
#16246 = EDGE_CURVE ( 'NONE', #17150, #410, #28346, .T. ) ;
#16245 = ORIENTED_EDGE ( 'NONE', *, *, #16317, .F. ) ;
#16247 = CIRCLE ( 'NONE', #22663, 64.76834224489934400 ) ;
#16248 = PLANE ( 'NONE',  #12048 ) ;
#16249 = CARTESIAN_POINT ( 'NONE',  ( -81.44467526201103169, 136.3898447976469868, 13.49545388103471311 ) ) ;
#16250 = VERTEX_POINT ( 'NONE', #26345 ) ;
#16251 = ADVANCED_FACE ( 'NONE', ( #10993 ), #12819, .F. ) ;
#16252 = VECTOR ( 'NONE', #13432, 1000.000000000000000 ) ;
#16253 = ORIENTED_EDGE ( 'NONE', *, *, #25377, .T. ) ;
#16254 = CARTESIAN_POINT ( 'NONE',  ( 139.9999999999999716, -120.0000000000000568, -100.0000000000000142 ) ) ;
#16255 = DIRECTION ( 'NONE',  ( -0.3897722486529259234, 0.9209112846414913012, 7.576567266530214112E-17 ) ) ;
#16256 = CARTESIAN_POINT ( 'NONE',  ( -71.37541315349507443, 230.0000000000000000, -5.000000000000002665 ) ) ;
#16257 = CARTESIAN_POINT ( 'NONE',  ( 99.01629842454553909, 234.2218078846129856, -21.79257675089547064 ) ) ;
#16258 = PLANE ( 'NONE',  #19955 ) ;
#16259 = DIRECTION ( 'NONE',  ( -1.000000000000000000, -8.673617379884036705E-17, -0.000000000000000000 ) ) ;
#16260 = CARTESIAN_POINT ( 'NONE',  ( -206.2579005266799186, 60.21847207785817346, -20.52143262683453528 ) ) ;
#16261 = VECTOR ( 'NONE', #13935, 999.9999999999998863 ) ;
#16262 = DIRECTION ( 'NONE',  ( -0.8916010070295011802, -0.4528218681379903021, 0.000000000000000000 ) ) ;
#16263 = DIRECTION ( 'NONE',  ( -1.000000000000000000, -0.000000000000000000, -0.000000000000000000 ) ) ;
#16264 = CARTESIAN_POINT ( 'NONE',  ( 134.9999999999998579, 220.0000000000000284, -105.0000000000000284 ) ) ;
#16265 = CIRCLE ( 'NONE', #3857, 5.000000000000004441 ) ;
#16266 = DIRECTION ( 'NONE',  ( -2.775557561562887407E-16, -3.668437989309015850E-32, 1.000000000000000000 ) ) ;
#16267 = ORIENTED_EDGE ( 'NONE', *, *, #26865, .T. ) ;
#16268 = CARTESIAN_POINT ( 'NONE',  ( -279.3160071107327553, -91.18033988749901653, 14.13483123440684253 ) ) ;
#16269 = CARTESIAN_POINT ( 'NONE',  ( -233.3699482038331610, 66.30323757540675444, 6.318463073150136999 ) ) ;
#16270 = DIRECTION ( 'NONE',  ( 0.000000000000000000, 0.000000000000000000, 1.000000000000000000 ) ) ;
#16271 = ORIENTED_EDGE ( 'NONE', *, *, #7015, .T. ) ;
#16272 = CARTESIAN_POINT ( 'NONE',  ( 238.4999999999996305, 133.0668745871126930, -36.86484227207694886 ) ) ;
#16274 = VERTEX_POINT ( 'NONE', #6675 ) ;
#16273 = EDGE_CURVE ( 'NONE', #15896, #26994, #5907, .T. ) ;
#16275 = EDGE_CURVE ( 'NONE', #8411, #22091, #11929, .T. ) ;
#16276 =( REPRESENTATION_RELATIONSHIP ('NONE','NONE', #11963, #13220 ) REPRESENTATION_RELATIONSHIP_WITH_TRANSFORMATION ( #3734 )SHAPE_REPRESENTATION_RELATIONSHIP( ) );
#16277 = CARTESIAN_POINT ( 'NONE',  ( 157.4999999999996874, 268.9035626463865469, 45.00000000000000000 ) ) ;
#16278 = FACE_OUTER_BOUND ( 'NONE', #25907, .T. ) ;
#16279 = ORIENTED_EDGE ( 'NONE', *, *, #18408, .F. ) ;
#16280 = VECTOR ( 'NONE', #5216, 1000.000000000000000 ) ;
#16281 = ORIENTED_EDGE ( 'NONE', *, *, #11591, .F. ) ;
#16282 = FACE_OUTER_BOUND ( 'NONE', #4694, .T. ) ;
#16283 = LINE ( 'NONE', #20574, #11189 ) ;
#16284 = LINE ( 'NONE', #25450, #8201 ) ;
#16285 = ORIENTED_EDGE ( 'NONE', *, *, #11995, .F. ) ;
#16286 = CARTESIAN_POINT ( 'NONE',  ( -48.38593899427829115, 148.2549133597845241, -45.00000000000000000 ) ) ;
#16287 = VERTEX_POINT ( 'NONE', #27334 ) ;
#16288 = AXIS2_PLACEMENT_3D ( 'NONE', #14600, #25644, #16479 ) ;
#16289 = CARTESIAN_POINT ( 'NONE',  ( -115.3221550338875687, 66.54464929955099706, 83.00000000000001421 ) ) ;
#16290 = LINE ( 'NONE', #24617, #9453 ) ;
#16291 = CARTESIAN_POINT ( 'NONE',  ( 176.5942101292460222, 101.9567147554491271, 45.00000000000000000 ) ) ;
#16292 = CARTESIAN_POINT ( 'NONE',  ( -13.31932916636724151, 129.6218899819808144, -16.84828668634186499 ) ) ;
#16293 = DIRECTION ( 'NONE',  ( -0.000000000000000000, 1.000000000000000000, -1.387778780781445429E-16 ) ) ;
#16294 = DIRECTION ( 'NONE',  ( -0.8916010070293783896, 0.4528218681382319422, 0.000000000000000000 ) ) ;
#16295 = CARTESIAN_POINT ( 'NONE',  ( 162.9441897050832893, 209.0821077902480170, -141.0313312019551972 ) ) ;
#16296 = ORIENTED_EDGE ( 'NONE', *, *, #21218, .F. ) ;
#16297 = EDGE_CURVE ( 'NONE', #11332, #19790, #7539, .T. ) ;
#16298 = LINE ( 'NONE', #25052, #9570 ) ;
#16299 = VECTOR ( 'NONE', #25768, 1000.000000000000000 ) ;
#16300 = CARTESIAN_POINT ( 'NONE',  ( 187.4999999999996305, 83.06687458711267880, -30.86484227207694886 ) ) ;
#16301 = CARTESIAN_POINT ( 'NONE',  ( 157.9999999999998295, 226.5236250225210313, 45.00000000000000000 ) ) ;
#16302 = ORIENTED_EDGE ( 'NONE', *, *, #9337, .T. ) ;
#16303 = AXIS2_PLACEMENT_3D ( 'NONE', #6598, #17795, #9185 ) ;
#16304 = CARTESIAN_POINT ( 'NONE',  ( -238.3976651326582044, 69.81518760999661311, 5.405651710414779210 ) ) ;
#16305 = VERTEX_POINT ( 'NONE', #9552 ) ;
#16306 = DIRECTION ( 'NONE',  ( 0.5457381880580551847, -0.8379557447115634217, 0.000000000000000000 ) ) ;
#16307 = CARTESIAN_POINT ( 'NONE',  ( -217.0264852877946566, -91.18033988749901653, 0.000000000000000000 ) ) ;
#16308 = FACE_OUTER_BOUND ( 'NONE', #24508, .T. ) ;
#16309 = ORIENTED_EDGE ( 'NONE', *, *, #6502, .F. ) ;
#16310 = LINE ( 'NONE', #20742, #7889 ) ;
#16311 = EDGE_CURVE ( 'NONE', #24757, #28358, #14654, .T. ) ;
#16312 = AXIS2_PLACEMENT_3D ( 'NONE', #24206, #362, #6679 ) ;
#16313 = ORIENTED_EDGE ( 'NONE', *, *, #1180, .T. ) ;
#16314 = EDGE_CURVE ( 'NONE', #25995, #19755, #23366, .T. ) ;
#16315 = EDGE_CURVE ( 'NONE', #6262, #21673, #3206, .T. ) ;
#16316 = CYLINDRICAL_SURFACE ( 'NONE', #8337, 30.00000000000000000 ) ;
#16317 = EDGE_CURVE ( 'NONE', #12148, #24050, #4935, .T. ) ;
#16318 = CARTESIAN_POINT ( 'NONE',  ( 104.1955293147850199, 245.8507536825374871, 19.98755400232634116 ) ) ;
#16319 = EDGE_LOOP ( 'NONE', ( #3733, #10783 ) ) ;
#16320 = ORIENTED_EDGE ( 'NONE', *, *, #670, .F. ) ;
#16321 = LINE ( 'NONE', #26942, #1234 ) ;
#16322 = ORIENTED_EDGE ( 'NONE', *, *, #18057, .T. ) ;
#16323 = VECTOR ( 'NONE', #24189, 1000.000000000000000 ) ;
#16324 = ORIENTED_EDGE ( 'NONE', *, *, #13256, .T. ) ;
#16325 = VERTEX_POINT ( 'NONE', #15886 ) ;
#16326 = VECTOR ( 'NONE', #20628, 1000.000000000000000 ) ;
#16327 = AXIS2_PLACEMENT_3D ( 'NONE', #815, #2671, #18345 ) ;
#16328 = CARTESIAN_POINT ( 'NONE',  ( 158.0000000000009663, 113.6692496847042264, 45.00000000000000000 ) ) ;
#16329 = LINE ( 'NONE', #7417, #7124 ) ;
#16330 = CARTESIAN_POINT ( 'NONE',  ( 2.399999999999999911, -1.249999999999998890, -8.000000000000000000 ) ) ;
#16331 = CIRCLE ( 'NONE', #9905, 22.49999999999999289 ) ;
#16332 = CARTESIAN_POINT ( 'NONE',  ( 109.9999999999999147, 140.0000000000000000, -90.00000000000004263 ) ) ;
#16333 = DIRECTION ( 'NONE',  ( 0.000000000000000000, -1.000000000000000000, 0.000000000000000000 ) ) ;
#16334 = CARTESIAN_POINT ( 'NONE',  ( 158.0000000000000853, 198.4291249324366504, 45.00000000000000000 ) ) ;
#16335 = DIRECTION ( 'NONE',  ( -0.000000000000000000, -0.000000000000000000, 1.000000000000000000 ) ) ;
#16336 = CARTESIAN_POINT ( 'NONE',  ( 167.4999999999996589, 494.4107529906318632, -74.99999999999995737 ) ) ;
#16337 = LINE ( 'NONE', #25086, #22862 ) ;
#16338 = CARTESIAN_POINT ( 'NONE',  ( -70.31278697424053803, 101.4626071723526195, -137.4901433416540328 ) ) ;
#16339 = ORIENTED_EDGE ( 'NONE', *, *, #9211, .T. ) ;
#16340 = EDGE_CURVE ( 'NONE', #23830, #5272, #2933, .T. ) ;
#16341 = EDGE_CURVE ( 'NONE', #13033, #14756, #26106, .T. ) ;
#16342 = EDGE_CURVE ( 'NONE', #194, #27280, #13727, .T. ) ;
#16343 = DIRECTION ( 'NONE',  ( 1.000000000000000000, 0.000000000000000000, 0.000000000000000000 ) ) ;
#16344 = DIRECTION ( 'NONE',  ( 0.8379557447115515423, -0.5457381880580733924, 0.000000000000000000 ) ) ;
#16345 = AXIS2_PLACEMENT_3D ( 'NONE', #21962, #24403, #24262 ) ;
#16346 = CARTESIAN_POINT ( 'NONE',  ( -248.1546605714623013, -91.18033988749901653, 0.000000000000000000 ) ) ;
#16347 = ORIENTED_EDGE ( 'NONE', *, *, #1879, .T. ) ;
#16348 = VECTOR ( 'NONE', #2086, 1000.000000000000000 ) ;
#16349 = DIRECTION ( 'NONE',  ( 0.9711705445023437466, -0.2383857661250380899, 0.000000000000000000 ) ) ;
#16350 = EDGE_LOOP ( 'NONE', ( #10789, #18103, #8311, #26006 ) ) ;
#16351 = EDGE_CURVE ( 'NONE', #10474, #12013, #3348, .T. ) ;
#16352 = LINE ( 'NONE', #13775, #12781 ) ;
#16353 = AXIS2_PLACEMENT_3D ( 'NONE', #22395, #13359, #10912 ) ;
#16354 = ORIENTED_EDGE ( 'NONE', *, *, #5060, .F. ) ;
#16355 = ORIENTED_EDGE ( 'NONE', *, *, #3116, .T. ) ;
#16356 = ORIENTED_EDGE ( 'NONE', *, *, #14742, .T. ) ;
#16357 = ORIENTED_EDGE ( 'NONE', *, *, #19988, .T. ) ;
#16358 = CARTESIAN_POINT ( 'NONE',  ( -122.9450662303175363, 132.7613262207298703, 14.33664937305252707 ) ) ;
#16359 = CARTESIAN_POINT ( 'NONE',  ( -17.24491960465745777, 0.000000000000000000, 95.00000000000000000 ) ) ;
#16360 = CARTESIAN_POINT ( 'NONE',  ( 157.4999999999998579, 220.0000000000000284, -105.0000000000000284 ) ) ;
#16361 = DIRECTION ( 'NONE',  ( 0.4528218681378515797, 0.8916010070295715684, -0.000000000000000000 ) ) ;
#16362 = VECTOR ( 'NONE', #5024, 1000.000000000000000 ) ;
#16363 = CARTESIAN_POINT ( 'NONE',  ( -5.421010862427522170E-17, 0.000000000000000000, 0.000000000000000000 ) ) ;
#16364 = CARTESIAN_POINT ( 'NONE',  ( -207.8278798888169945, 75.36218601466582356, 41.22349376586717540 ) ) ;
#16365 = CARTESIAN_POINT ( 'NONE',  ( 158.0000000000008811, 121.1928747072253572, -45.00000000000000000 ) ) ;
#16366 = CARTESIAN_POINT ( 'NONE',  ( 158.0000000000010232, 106.1456246621830957, 45.00000000000000000 ) ) ;
#16367 = DIRECTION ( 'NONE',  ( 0.9659258262890670910, -0.2588190451025251804, 0.000000000000000000 ) ) ;
#16368 = CARTESIAN_POINT ( 'NONE',  ( -230.7999239170523538, 92.53513801463330424, -13.02866169270885344 ) ) ;
#16369 = VECTOR ( 'NONE', #4365, 1000.000000000000114 ) ;
#16370 = CARTESIAN_POINT ( 'NONE',  ( 134.9999999999998579, 244.8793018922092699, -145.0000000000000000 ) ) ;
#16371 = LINE ( 'NONE', #20948, #6322 ) ;
#16372 = LINE ( 'NONE', #27538, #24438 ) ;
#16373 = ORIENTED_EDGE ( 'NONE', *, *, #7934, .F. ) ;
#16374 = EDGE_CURVE ( 'NONE', #9499, #7395, #9689, .T. ) ;
#16375 = LINE ( 'NONE', #16096, #16952 ) ;
#16376 = DIRECTION ( 'NONE',  ( 0.000000000000000000, -1.000000000000000000, 0.000000000000000000 ) ) ;
#16377 = FACE_OUTER_BOUND ( 'NONE', #2610, .T. ) ;
#16379 = ORIENTED_EDGE ( 'NONE', *, *, #7865, .T. ) ;
#16378 = EDGE_LOOP ( 'NONE', ( #24998, #2747, #22670, #9254 ) ) ;
#16380 = LINE ( 'NONE', #16655, #24893 ) ;
#16381 = ORIENTED_EDGE ( 'NONE', *, *, #11115, .F. ) ;
#16382 = VERTEX_POINT ( 'NONE', #18025 ) ;
#16383 = VECTOR ( 'NONE', #22643, 1000.000000000000227 ) ;
#16384 = ORIENTED_EDGE ( 'NONE', *, *, #24281, .T. ) ;
#16385 = EDGE_CURVE ( 'NONE', #5481, #10749, #1062, .T. ) ;
#16386 = ADVANCED_FACE ( 'NONE', ( #12139 ), #18173, .T. ) ;
#16387 = VERTEX_POINT ( 'NONE', #9829 ) ;
#16388 = EDGE_LOOP ( 'NONE', ( #22281, #11597, #23151, #4664 ) ) ;
#16389 = DIRECTION ( 'NONE',  ( -0.8916010070299471568, 0.4528218681371123377, 0.000000000000000000 ) ) ;
#16390 = LINE ( 'NONE', #12082, #25124 ) ;
#16391 = CARTESIAN_POINT ( 'NONE',  ( 0.3651377029009472142, 1.249999999999999556, 7.402212548643259282 ) ) ;
#16392 = CARTESIAN_POINT ( 'NONE',  ( 95.14887760048110010, 231.7800724511707813, -19.10096717460264770 ) ) ;
#16393 = EDGE_CURVE ( 'NONE', #1795, #26789, #11719, .T. ) ;
#16394 = DIRECTION ( 'NONE',  ( -0.000000000000000000, -0.000000000000000000, 1.000000000000000000 ) ) ;
#16395 = EDGE_CURVE ( 'NONE', #2018, #12452, #26926, .T. ) ;
#16396 = DIRECTION ( 'NONE',  ( 0.000000000000000000, -1.000000000000000000, 0.000000000000000000 ) ) ;
#16397 = PLANE ( 'NONE',  #2631 ) ;
#16398 = VECTOR ( 'NONE', #20544, 1000.000000000000114 ) ;
#16399 = CARTESIAN_POINT ( 'NONE',  ( -194.2478650485211062, 63.21120109188145619, -44.02102422013626892 ) ) ;
#16400 = CARTESIAN_POINT ( 'NONE',  ( 111.0430938661146030, 201.9396954599693572, -140.2311020877163514 ) ) ;
#16401 = ADVANCED_BREP_SHAPE_REPRESENTATION ( '', ( #27970, #10637 ), #7887 ) ;
#16402 = LINE ( 'NONE', #5611, #22988 ) ;
#16403 = DIRECTION ( 'NONE',  ( -0.000000000000000000, -0.000000000000000000, 1.000000000000000000 ) ) ;
#16404 = CARTESIAN_POINT ( 'NONE',  ( 157.4999999999998579, 158.5570623160774630, 45.00000000000000000 ) ) ;
#16405 = ORIENTED_EDGE ( 'NONE', *, *, #15206, .F. ) ;
#16406 = LINE ( 'NONE', #4762, #24770 ) ;
#16407 = CARTESIAN_POINT ( 'NONE',  ( -235.5446291276685713, 67.70753763449820894, 5.872244511703956782 ) ) ;
#16408 = FACE_OUTER_BOUND ( 'NONE', #13375, .T. ) ;
#16409 = ORIENTED_EDGE ( 'NONE', *, *, #13635, .T. ) ;
#16410 = DIRECTION ( 'NONE',  ( 1.000000000000000000, 0.000000000000000000, 0.000000000000000000 ) ) ;
#16411 = VERTEX_POINT ( 'NONE', #3065 ) ;
#16412 = CIRCLE ( 'NONE', #4069, 30.00000000000000000 ) ;
#16413 = EDGE_CURVE ( 'NONE', #7931, #23684, #501, .T. ) ;
#16414 = CARTESIAN_POINT ( 'NONE',  ( 232.4999999999996305, 83.06687458711267880, 30.83984227207693607 ) ) ;
#16415 = CARTESIAN_POINT ( 'NONE',  ( 0.3651377029009472142, 1.249999999999999556, 7.402212548643259282 ) ) ;
#16416 = ORIENTED_EDGE ( 'NONE', *, *, #7465, .T. ) ;
#16417 = AXIS2_PLACEMENT_3D ( 'NONE', #7161, #24685, #13785 ) ;
#16418 = ORIENTED_EDGE ( 'NONE', *, *, #26021, .F. ) ;
#16419 = DIRECTION ( 'NONE',  ( -0.000000000000000000, -0.000000000000000000, -1.000000000000000000 ) ) ;
#16420 = DIRECTION ( 'NONE',  ( 0.000000000000000000, 0.000000000000000000, 1.000000000000000000 ) ) ;
#16421 = LINE ( 'NONE', #5207, #27909 ) ;
#16422 = EDGE_LOOP ( 'NONE', ( #20899, #17493, #22943, #16754 ) ) ;
#16423 = CARTESIAN_POINT ( 'NONE',  ( 82.91040908012763566, 80.00000000660637056, 100.0000000000000142 ) ) ;
#16424 = ORIENTED_EDGE ( 'NONE', *, *, #18501, .F. ) ;
#16425 = LINE ( 'NONE', #906, #18039 ) ;
#16426 = CARTESIAN_POINT ( 'NONE',  ( 158.0000000000000284, 203.9527499549551806, 45.00000000000000000 ) ) ;
#16427 = CARTESIAN_POINT ( 'NONE',  ( 157.9999999999998010, 231.5393750375350237, 45.00000000000000000 ) ) ;
#16428 = FACE_OUTER_BOUND ( 'NONE', #10233, .T. ) ;
#16429 = LINE ( 'NONE', #5497, #26093 ) ;
#16430 = ADVANCED_FACE ( 'NONE', ( #8374 ), #12418, .F. ) ;
#16431 = EDGE_CURVE ( 'NONE', #6317, #12327, #27891, .T. ) ;
#16432 = CARTESIAN_POINT ( 'NONE',  ( 157.9999999999996305, 286.7126252026890256, -45.00000000000000000 ) ) ;
#16433 = PLANE ( 'NONE',  #5127 ) ;
#16434 = CONICAL_SURFACE ( 'NONE', #27417, 6.025000000000002132, 0.7853981633974482790 ) ;
#16435 = VERTEX_POINT ( 'NONE', #19288 ) ;
#16436 = FACE_OUTER_BOUND ( 'NONE', #15150, .T. ) ;
#16437 = EDGE_CURVE ( 'NONE', #18588, #10524, #1619, .T. ) ;
#16438 = DIRECTION ( 'NONE',  ( -0.7440215159218956931, 0.6681556583950213346, 0.000000000000000000 ) ) ;
#16439 = DIRECTION ( 'NONE',  ( 0.000000000000000000, -1.000000000000000000, 0.000000000000000000 ) ) ;
#16440 = ORIENTED_EDGE ( 'NONE', *, *, #11615, .F. ) ;
#16441 = DIRECTION ( 'NONE',  ( 0.000000000000000000, 0.000000000000000000, -1.000000000000000000 ) ) ;
#16442 = ORIENTED_EDGE ( 'NONE', *, *, #13381, .T. ) ;
#16443 = DIRECTION ( 'NONE',  ( -0.8916010070298868717, -0.4528218681372309651, 0.000000000000000000 ) ) ;
#16444 = LINE ( 'NONE', #14152, #19267 ) ;
#16445 = DIRECTION ( 'NONE',  ( -0.8916010070295616874, -0.4528218681378710642, 0.000000000000000000 ) ) ;
#16446 = VERTEX_POINT ( 'NONE', #27753 ) ;
#16447 = DIRECTION ( 'NONE',  ( -0.000000000000000000, 1.000000000000000000, -1.387778780781445429E-16 ) ) ;
#16448 = SURFACE_STYLE_USAGE ( .BOTH. , #11726 ) ;
#16449 = ORIENTED_EDGE ( 'NONE', *, *, #15507, .T. ) ;
#16450 = LINE ( 'NONE', #27073, #17516 ) ;
#16451 = CYLINDRICAL_SURFACE ( 'NONE', #9456, 5.999999999999977796 ) ;
#16452 = EDGE_LOOP ( 'NONE', ( #11325, #4796, #20247, #12502 ) ) ;
#16453 = VERTEX_POINT ( 'NONE', #14426 ) ;
#16454 = CARTESIAN_POINT ( 'NONE',  ( 158.0000000000012221, 90.59049960963380954, 45.00000000000000000 ) ) ;
#16455 = ORIENTED_EDGE ( 'NONE', *, *, #14985, .F. ) ;
#16456 = VECTOR ( 'NONE', #26956, 1000.000000000000000 ) ;
#16457 = AXIS2_PLACEMENT_3D ( 'NONE', #20871, #9251, #25179 ) ;
#16458 = VERTEX_POINT ( 'NONE', #19144 ) ;
#16459 = ORIENTED_EDGE ( 'NONE', *, *, #20062, .T. ) ;
#16460 = FACE_OUTER_BOUND ( 'NONE', #18008, .T. ) ;
#16461 = CARTESIAN_POINT ( 'NONE',  ( -216.6285223362424404, 139.2238150404710666, 13.00000000000000178 ) ) ;
#16462 = EDGE_CURVE ( 'NONE', #12635, #9863, #2635, .T. ) ;
#16463 = CARTESIAN_POINT ( 'NONE',  ( 232.4749999999995964, 133.0668745871126930, -36.86484227207694886 ) ) ;
#16464 = EDGE_CURVE ( 'NONE', #4054, #8160, #5654, .T. ) ;
#16465 = CARTESIAN_POINT ( 'NONE',  ( 87.74278500246884960, 111.0010834413659921, -71.13281249983540988 ) ) ;
#16466 = DIRECTION ( 'NONE',  ( 0.000000000000000000, 0.000000000000000000, 1.000000000000000000 ) ) ;
#16467 = CARTESIAN_POINT ( 'NONE',  ( 157.4999999999996874, 266.3956876388795649, 45.00000000000000000 ) ) ;
#16468 = VECTOR ( 'NONE', #13654, 1000.000000000000000 ) ;
#16469 = EDGE_CURVE ( 'NONE', #10091, #17968, #19225, .T. ) ;
#16470 = CARTESIAN_POINT ( 'NONE',  ( 134.1167547769962596, -7.205103435269982093, -45.00000000000000000 ) ) ;
#16471 = CARTESIAN_POINT ( 'NONE',  ( 113.4999999999998863, 220.0000000000000284, 100.0000000000000142 ) ) ;
#16472 = FACE_OUTER_BOUND ( 'NONE', #13392, .T. ) ;
#16473 = DIRECTION ( 'NONE',  ( 1.000000000000000000, 0.000000000000000000, -0.000000000000000000 ) ) ;
#16474 = EDGE_LOOP ( 'NONE', ( #6441, #9806 ) ) ;
#16475 = CARTESIAN_POINT ( 'NONE',  ( -8.960146631618641777, 132.3429123680572275, 14.45742179905339952 ) ) ;
#16476 = CIRCLE ( 'NONE', #3142, 67.21503689626328537 ) ;
#16477 = CIRCLE ( 'NONE', #20129, 5.999999999999977796 ) ;
#16478 = CARTESIAN_POINT ( 'NONE',  ( 104.1954684636752972, 245.8506931952819627, -19.98744076451168183 ) ) ;
#16479 = DIRECTION ( 'NONE',  ( 0.000000000000000000, 0.000000000000000000, -1.000000000000000000 ) ) ;
#16480 = CARTESIAN_POINT ( 'NONE',  ( 158.0000000000010232, 108.1456246621830957, -45.00000000000000000 ) ) ;
#16481 = ORIENTED_EDGE ( 'NONE', *, *, #27114, .F. ) ;
#16482 = AXIS2_PLACEMENT_3D ( 'NONE', #25871, #4173, #23722 ) ;
#16483 = FACE_OUTER_BOUND ( 'NONE', #16100, .T. ) ;
#16484 = EDGE_LOOP ( 'NONE', ( #661, #23885, #22275, #18172 ) ) ;
#16485 = DIRECTION ( 'NONE',  ( 0.000000000000000000, 9.486769009248162565E-17, -1.000000000000000000 ) ) ;
#16486 = ORIENTED_EDGE ( 'NONE', *, *, #11480, .T. ) ;
#16487 = VERTEX_POINT ( 'NONE', #17135 ) ;
#16488 = AXIS2_PLACEMENT_3D ( 'NONE', #2784, #647, #16162 ) ;
#16489 = ORIENTED_EDGE ( 'NONE', *, *, #3145, .F. ) ;
#16490 = VECTOR ( 'NONE', #9362, 1000.000000000000000 ) ;
#16491 = EDGE_LOOP ( 'NONE', ( #19777, #4474 ) ) ;
#16492 = ORIENTED_EDGE ( 'NONE', *, *, #5750, .F. ) ;
#16493 = CARTESIAN_POINT ( 'NONE',  ( 114.6895484223571771, 229.7318084278312540, 98.48649515991442627 ) ) ;
#16494 = CARTESIAN_POINT ( 'NONE',  ( -212.2419371577844345, -220.0000000000000853, -94.99999999999987210 ) ) ;
#16495 = EDGE_CURVE ( 'NONE', #15548, #13125, #16578, .T. ) ;
#16496 = VECTOR ( 'NONE', #14498, 1000.000000000000000 ) ;
#16497 = ADVANCED_FACE ( 'NONE', ( #25891, #23457 ), #18863, .F. ) ;
#16498 = CARTESIAN_POINT ( 'NONE',  ( -92.74993325912653575, 136.3626345347758502, -13.50003192765508508 ) ) ;
#16499 = CIRCLE ( 'NONE', #21998, 6.025000000000002132 ) ;
#16500 = EDGE_CURVE ( 'NONE', #24747, #16964, #5792, .T. ) ;
#16501 = DIRECTION ( 'NONE',  ( -0.000000000000000000, -0.000000000000000000, -1.000000000000000000 ) ) ;
#16502 = PLANE ( 'NONE',  #15081 ) ;
#16503 = FACE_OUTER_BOUND ( 'NONE', #5939, .T. ) ;
#16504 = EDGE_CURVE ( 'NONE', #5960, #230, #15564, .T. ) ;
#16505 = CARTESIAN_POINT ( 'NONE',  ( 134.2176099750896583, 249.9923178888783752, -139.0380470571626574 ) ) ;
#16506 = CARTESIAN_POINT ( 'NONE',  ( -268.8075929731044766, -170.5243996965605504, -94.03848302756206579 ) ) ;
#16507 = DIRECTION ( 'NONE',  ( -0.000000000000000000, -1.000000000000000000, -0.000000000000000000 ) ) ;
#16508 = CARTESIAN_POINT ( 'NONE',  ( 232.4999999999996305, 133.0668745871126930, -36.86484227207694886 ) ) ;
#16509 = CARTESIAN_POINT ( 'NONE',  ( 104.9999999999998579, 220.0000000000000284, -122.9999999999999574 ) ) ;
#16510 = ORIENTED_EDGE ( 'NONE', *, *, #8219, .F. ) ;
#16511 = CARTESIAN_POINT ( 'NONE',  ( -241.9743096803475453, -91.18033988749901653, 17.46154499483315448 ) ) ;
#16512 = CARTESIAN_POINT ( 'NONE',  ( 158.0000000000013074, 83.06687458711267880, -45.00000000000000000 ) ) ;
#16513 = LINE ( 'NONE', #21476, #11621 ) ;
#16515 = ORIENTED_EDGE ( 'NONE', *, *, #2899, .T. ) ;
#16514 = ORIENTED_EDGE ( 'NONE', *, *, #24444, .T. ) ;
#16516 = AXIS2_PLACEMENT_3D ( 'NONE', #6851, #27099, #9728 ) ;
#16517 = CARTESIAN_POINT ( 'NONE',  ( 139.9869122110690114, 197.5248869502487139, 45.00000000000000000 ) ) ;
#16518 = VERTEX_POINT ( 'NONE', #14992 ) ;
#16519 = ORIENTED_EDGE ( 'NONE', *, *, #11648, .T. ) ;
#16520 = AXIS2_PLACEMENT_3D ( 'NONE', #21759, #21893, #2065 ) ;
#16521 = ORIENTED_EDGE ( 'NONE', *, *, #21821, .F. ) ;
#16522 = ORIENTED_EDGE ( 'NONE', *, *, #26341, .T. ) ;
#16523 = EDGE_CURVE ( 'NONE', #18620, #2585, #21014, .T. ) ;
#16524 = VERTEX_POINT ( 'NONE', #9966 ) ;
#16525 = CARTESIAN_POINT ( 'NONE',  ( 134.9999999999998579, 220.0000000000000284, -189.9999999999999716 ) ) ;
#16526 = FACE_OUTER_BOUND ( 'NONE', #24290, .T. ) ;
#16527 = EDGE_CURVE ( 'NONE', #17634, #16387, #18725, .T. ) ;
#16528 = VECTOR ( 'NONE', #21927, 1000.000000000000114 ) ;
#16529 = DIRECTION ( 'NONE',  ( 1.000000000000000000, 0.000000000000000000, 0.000000000000000000 ) ) ;
#16530 = CARTESIAN_POINT ( 'NONE',  ( 158.0000000000006537, 143.7637497747887210, -45.00000000000000000 ) ) ;
#16531 = AXIS2_PLACEMENT_3D ( 'NONE', #9556, #20321, #20176 ) ;
#16532 = CARTESIAN_POINT ( 'NONE',  ( 158.0000000000006537, 141.2558747672816821, 45.00000000000000000 ) ) ;
#16533 = EDGE_CURVE ( 'NONE', #18280, #8829, #10112, .T. ) ;
#16534 = DIRECTION ( 'NONE',  ( -0.8916010070296632728, -0.4528218681376712240, 0.000000000000000000 ) ) ;
#16535 = CARTESIAN_POINT ( 'NONE',  ( 157.9999999999998579, 219.0000000000000284, 45.00000000000000000 ) ) ;
#16536 = CARTESIAN_POINT ( 'NONE',  ( -209.7353312573863207, 74.09610071451170654, -35.01412046639265441 ) ) ;
#16537 = EDGE_CURVE ( 'NONE', #9050, #7851, #14564, .T. ) ;
#16538 = CARTESIAN_POINT ( 'NONE',  ( 112.2863758723266727, 200.4016019532060113, -142.8785553633036898 ) ) ;
#16539 = LINE ( 'NONE', #12240, #6922 ) ;
#16540 = DIRECTION ( 'NONE',  ( 0.000000000000000000, 0.000000000000000000, -1.000000000000000000 ) ) ;
#16541 = ORIENTED_EDGE ( 'NONE', *, *, #16850, .T. ) ;
#16542 = CARTESIAN_POINT ( 'NONE',  ( 119.1208832861758538, 235.9842039383417784, -100.0000000000002842 ) ) ;
#16543 = VECTOR ( 'NONE', #7132, 1000.000000000000000 ) ;
#16544 = CARTESIAN_POINT ( 'NONE',  ( -40.00387671809203738, 149.2965004116384762, 45.00000000000000000 ) ) ;
#16545 = ORIENTED_EDGE ( 'NONE', *, *, #24211, .F. ) ;
#16546 = ORIENTED_EDGE ( 'NONE', *, *, #18181, .F. ) ;
#16547 = EDGE_CURVE ( 'NONE', #24909, #9062, #27612, .T. ) ;
#16548 = ORIENTED_EDGE ( 'NONE', *, *, #15435, .T. ) ;
#16549 = CIRCLE ( 'NONE', #21583, 24.07986109634097005 ) ;
#16550 = FACE_OUTER_BOUND ( 'NONE', #6053, .T. ) ;
#16551 = CARTESIAN_POINT ( 'NONE',  ( 119.4436508138957720, 236.9705627484767376, 45.00000000000000000 ) ) ;
#16552 = ORIENTED_EDGE ( 'NONE', *, *, #6073, .T. ) ;
#16553 = ORIENTED_EDGE ( 'NONE', *, *, #14624, .T. ) ;
#16554 = CARTESIAN_POINT ( 'NONE',  ( 158.0000000000006253, 148.2716247822957882, -45.00000000000000000 ) ) ;
#16555 = EDGE_CURVE ( 'NONE', #26681, #26218, #26553, .T. ) ;
#16556 = DIRECTION ( 'NONE',  ( 0.4528218681372709331, -0.8916010070298664436, 0.000000000000000000 ) ) ;
#16557 = DIRECTION ( 'NONE',  ( -1.000000000000000000, 0.000000000000000000, 0.000000000000000000 ) ) ;
#16558 = ORIENTED_EDGE ( 'NONE', *, *, #26274, .F. ) ;
#16559 = PLANE ( 'NONE',  #27942 ) ;
#16560 = ORIENTED_EDGE ( 'NONE', *, *, #9659, .F. ) ;
#16561 = CARTESIAN_POINT ( 'NONE',  ( 130.0130877889311591, 197.5248869502486571, -45.00000000000000000 ) ) ;
#16562 = AXIS2_PLACEMENT_3D ( 'NONE', #21573, #15269, #7027 ) ;
#16563 = CARTESIAN_POINT ( 'NONE',  ( -55.40193461144291831, 169.7519813918499665, -45.00000000000000000 ) ) ;
#16564 = CARTESIAN_POINT ( 'NONE',  ( 109.9999999999999432, 140.0000000000000000, -99.99999999999998579 ) ) ;
#16565 = CARTESIAN_POINT ( 'NONE',  ( 65.00000000000000000, -120.0000000000000995, -63.97499999999998721 ) ) ;
#16566 = CARTESIAN_POINT ( 'NONE',  ( 157.4999999999997726, 243.8248125713165280, 45.00000000000000000 ) ) ;
#16567 = EDGE_CURVE ( 'NONE', #16772, #12468, #1343, .T. ) ;
#16568 = LINE ( 'NONE', #12692, #20227 ) ;
#16569 = VECTOR ( 'NONE', #20416, 1000.000000000000000 ) ;
#16570 = CARTESIAN_POINT ( 'NONE',  ( 158.0000000000017053, 45.44874947450702507, 45.00000000000000000 ) ) ;
#16571 = ORIENTED_EDGE ( 'NONE', *, *, #23856, .F. ) ;
#16572 = EDGE_CURVE ( 'NONE', #12431, #19970, #1894, .T. ) ;
#16573 = LINE ( 'NONE', #3621, #847 ) ;
#16574 = CARTESIAN_POINT ( 'NONE',  ( 158.0000000000012506, 86.08262460212675649, 45.00000000000000000 ) ) ;
#16575 = CARTESIAN_POINT ( 'NONE',  ( 158.0000000000012221, 90.59049960963380954, -45.00000000000000000 ) ) ;
#16576 = CARTESIAN_POINT ( 'NONE',  ( 157.9999999999999432, 211.4763749774776045, -45.00000000000000000 ) ) ;
#16577 = VERTEX_POINT ( 'NONE', #26445 ) ;
#16578 = LINE ( 'NONE', #3913, #7321 ) ;
#16579 = EDGE_LOOP ( 'NONE', ( #14511, #23353, #15823, #6862, #648, #14644, #25803, #25243, #6154, #14539, #18149, #15388, #6656, #22767, #27439, #4911, #12595, #9090, #19818, #26363, #12850, #11556, #5585, #18356, #17809, #26762, #3465, #15452, #21661, #4913, #8060, #49, #14540, #20067, #23312, #11040, #16657, #18727, #24506, #8215, #11975, #27543, #357, #12811, #25547, #27112, #25722, #934, #23341, #652, #6258, #13670, #8024, #8139, #8394, #22605, #4, #27379, #27382, #7413, #6211, #25329, #252, #24165, #14432, #5191, #17250, #15216, #14023, #10940, #9060, #18363, #16700, #5020, #16040, #11436, #85, #13027, #15286, #24676, #5899, #10934, #4754, #7672, #25619, #4556, #24725, #4987, #9394, #13665, #24025, #3788, #23363, #666, #1836, #23595, #28160, #24075, #21778, #33, #22202, #28081, #4640, #3570, #17701, #24988, #8033, #20640, #16213, #806, #21410, #3286, #10992, #25265, #18250, #26629, #13637, #9528, #20849, #19161, #18147, #22093, #12152, #1322, #28162, #26600, #13927, #8487, #10617, #12570, #27135, #4421, #23286, #19396, #5414, #10790, #12463, #5265, #9585, #17644, #12216, #27168, #10616, #19859, #5135, #11400, #2259, #2186, #5341, #20102, #3712, #21566, #8136, #15668, #20425, #13139, #14445, #20070, #15005, #28041, #110, #1857, #19449, #5966, #14789, #25408, #22977, #25018, #21283, #11737, #27647, #13276, #26179, #25072, #15718, #28068, #15904, #14197, #12919, #10442, #1562, #27869, #18249, #26396, #2350, #20025, #21060, #23173, #24342, #17243, #16899, #10251, #6578, #13956, #11988, #14466, #12072, #3181, #16042, #22897, #22207, #5386, #13629, #13923, #22412, #12574, #13777, #22194, #26559, #3320, #14785, #23474, #15926, #14782, #21382, #25101, #6476, #265, #10022, #27864, #14129, #6063, #21914, #15675, #25684, #23295, #27061, #5369, #2729, #5765, #15250, #2474, #8461, #19907, #27409, #26138, #5634, #27865, #18395, #6500, #22129, #17459, #17775, #10560, #15136, #5244, #5935, #15040, #6826, #20744, #1022, #3998, #14093, #14983, #3650, #2650, #17696, #18359, #23546, #23871, #24576, #229, #14633, #2300, #8569, #15067, #19750, #22642, #2215, #19709, #16132, #19259, #233, #12608, #11802, #27774, #21353, #4214, #20950, #19057, #22234, #10221, #5175, #15844, #12501, #4380, #26045, #12917, #1893, #8938, #10409, #19149, #11867, #8955, #7856, #6802, #24210, #28203, #24712, #25117 ) ) ;
#16580 = CARTESIAN_POINT ( 'NONE',  ( 185.9255560592262100, 121.0883471088020116, -45.00000000000000000 ) ) ;
#16581 = LINE ( 'NONE', #18590, #16992 ) ;
#16582 = CARTESIAN_POINT ( 'NONE',  ( 89.99999999999994316, -70.00000000000001421, -25.00000000000000000 ) ) ;
#16583 = ORIENTED_EDGE ( 'NONE', *, *, #17352, .F. ) ;
#16584 = LINE ( 'NONE', #7818, #18876 ) ;
#16585 = CARTESIAN_POINT ( 'NONE',  ( 158.0000000000007958, 130.7164997297464595, 45.00000000000000000 ) ) ;
#16586 = ORIENTED_EDGE ( 'NONE', *, *, #24297, .T. ) ;
#16587 = EDGE_CURVE ( 'NONE', #12172, #15969, #179, .T. ) ;
#16588 = AXIS2_PLACEMENT_3D ( 'NONE', #19461, #19174, #8408 ) ;
#16589 = CARTESIAN_POINT ( 'NONE',  ( 157.4999999999997442, 251.3484375938375024, 45.00000000000000000 ) ) ;
#16590 = DIRECTION ( 'NONE',  ( 0.000000000000000000, -1.000000000000000000, 0.000000000000000000 ) ) ;
#16591 = ORIENTED_EDGE ( 'NONE', *, *, #16495, .F. ) ;
#16592 = EDGE_CURVE ( 'NONE', #11585, #23433, #11244, .T. ) ;
#16593 = ORIENTED_EDGE ( 'NONE', *, *, #1564, .T. ) ;
#16594 = ADVANCED_FACE ( 'NONE', ( #6921, #23886 ), #19995, .F. ) ;
#16595 = CARTESIAN_POINT ( 'NONE',  ( 119.1329331941753225, 207.8247714198252254, 45.00000000000000000 ) ) ;
#16596 = EDGE_LOOP ( 'NONE', ( #14121, #762 ) ) ;
#16597 = ADVANCED_FACE ( 'NONE', ( #15279 ), #15700, .F. ) ;
#16598 = VERTEX_POINT ( 'NONE', #2040 ) ;
#16599 = ORIENTED_EDGE ( 'NONE', *, *, #25383, .T. ) ;
#16600 = CARTESIAN_POINT ( 'NONE',  ( 109.7119445821606121, 256.4759837302462984, 40.72317850545354645 ) ) ;
#16601 = CARTESIAN_POINT ( 'NONE',  ( -305.0000000000001137, -170.0000000000001137, -59.99999999999986500 ) ) ;
#16602 = CARTESIAN_POINT ( 'NONE',  ( -146.6428522700808230, 17.24192588826928585, 83.00000000000001421 ) ) ;
#16603 = FACE_OUTER_BOUND ( 'NONE', #9521, .T. ) ;
#16604 = LINE ( 'NONE', #23485, #10814 ) ;
#16605 = CARTESIAN_POINT ( 'NONE',  ( 157.4999999999997726, 246.3326875788235384, 45.00000000000000000 ) ) ;
#16606 = VECTOR ( 'NONE', #20311, 1000.000000000000000 ) ;
#16607 = CARTESIAN_POINT ( 'NONE',  ( -205.7061355896894383, 146.0477147645469813, -13.00000000000000000 ) ) ;
#16608 = EDGE_CURVE ( 'NONE', #2218, #6433, #9080, .T. ) ;
#16609 = CARTESIAN_POINT ( 'NONE',  ( -210.0000000000000568, -220.0000000000000853, 90.87829376371914236 ) ) ;
#16611 = DIRECTION ( 'NONE',  ( -0.000000000000000000, -0.000000000000000000, -1.000000000000000000 ) ) ;
#16610 = CIRCLE ( 'NONE', #18896, 11.00000000000001066 ) ;
#16612 = CARTESIAN_POINT ( 'NONE',  ( 119.1329331941753225, 207.8247714198252254, 45.00000000000000000 ) ) ;
#16613 = AXIS2_PLACEMENT_3D ( 'NONE', #9936, #27169, #25025 ) ;
#16614 = EDGE_LOOP ( 'NONE', ( #28298, #18113, #25791, #10919 ) ) ;
#16615 = CARTESIAN_POINT ( 'NONE',  ( 157.4999999999998579, 201.1909374436971802, 45.00000000000000000 ) ) ;
#16616 =( GEOMETRIC_REPRESENTATION_CONTEXT ( 3 ) GLOBAL_UNCERTAINTY_ASSIGNED_CONTEXT ( ( #5144 ) ) GLOBAL_UNIT_ASSIGNED_CONTEXT ( ( #26485, #9696, #18320 ) ) REPRESENTATION_CONTEXT ( 'NONE', 'WORKASPACE' ) );
#16617 = LINE ( 'NONE', #18621, #18361 ) ;
#16618 = LINE ( 'NONE', #27793, #27713 ) ;
#16619 = SURFACE_STYLE_USAGE ( .BOTH. , #21339 ) ;
#16620 = DIRECTION ( 'NONE',  ( 0.000000000000000000, 0.000000000000000000, -1.000000000000000000 ) ) ;
#16621 = ORIENTED_EDGE ( 'NONE', *, *, #16758, .F. ) ;
#16622 = LINE ( 'NONE', #21062, #25360 ) ;
#16623 = ORIENTED_EDGE ( 'NONE', *, *, #27676, .T. ) ;
#16624 = DIRECTION ( 'NONE',  ( 0.000000000000000000, -1.000000000000000000, 0.000000000000000000 ) ) ;
#16625 = ORIENTED_EDGE ( 'NONE', *, *, #816, .T. ) ;
#16626 = EDGE_CURVE ( 'NONE', #5554, #27204, #16930, .T. ) ;
#16627 = ORIENTED_EDGE ( 'NONE', *, *, #22981, .F. ) ;
#16628 = EDGE_CURVE ( 'NONE', #12668, #5675, #10672, .T. ) ;
#16629 = AXIS2_PLACEMENT_3D ( 'NONE', #1718, #12381, #18968 ) ;
#16630 = ORIENTED_EDGE ( 'NONE', *, *, #3981, .F. ) ;
#16631 = ORIENTED_EDGE ( 'NONE', *, *, #17505, .F. ) ;
#16632 = AXIS2_PLACEMENT_3D ( 'NONE', #586, #9352, #3144 ) ;
#16633 = CARTESIAN_POINT ( 'NONE',  ( 112.5174913703662014, 221.0249876999270953, 96.63436734148048401 ) ) ;
#16634 = DIRECTION ( 'NONE',  ( 0.000000000000000000, 0.000000000000000000, -1.000000000000000000 ) ) ;
#16635 = CARTESIAN_POINT ( 'NONE',  ( 340.3127869742386338, 101.4626071723496779, -152.5098566583459672 ) ) ;
#16636 = VECTOR ( 'NONE', #27545, 1000.000000000000000 ) ;
#16637 = DIRECTION ( 'NONE',  ( 1.000000000000000000, 0.000000000000000000, -0.000000000000000000 ) ) ;
#16638 = CARTESIAN_POINT ( 'NONE',  ( -197.4451421692467079, 62.05060586452424332, 32.13681025546651426 ) ) ;
#16639 = DIRECTION ( 'NONE',  ( 1.049727191138617093E-16, 0.5150380749100560429, -0.8571673007021111124 ) ) ;
#16640 = CARTESIAN_POINT ( 'NONE',  ( -82.58132619288578269, 136.4857224512149116, -13.47873422864532955 ) ) ;
#16641 = ADVANCED_FACE ( 'NONE', ( #21869, #12983 ), #26172, .T. ) ;
#16642 = FACE_OUTER_BOUND ( 'NONE', #16614, .T. ) ;
#16643 = CARTESIAN_POINT ( 'NONE',  ( -206.0012425902573909, 90.39787868968801376, 28.20958337426846541 ) ) ;
#16644 = DIRECTION ( 'NONE',  ( 0.4528218681382319422, -0.8916010070293783896, 0.000000000000000000 ) ) ;
#16645 = DIRECTION ( 'NONE',  ( 0.3102637045530753368, 0.9506505318133483540, -0.000000000000000000 ) ) ;
#16646 = EDGE_LOOP ( 'NONE', ( #8068, #13266 ) ) ;
#16647 = CIRCLE ( 'NONE', #4691, 6.000000000000005329 ) ;
#16648 = VECTOR ( 'NONE', #22696, 999.9999999999998863 ) ;
#16649 = EDGE_CURVE ( 'NONE', #26105, #8289, #12837, .T. ) ;
#16650 = CARTESIAN_POINT ( 'NONE',  ( -215.4886702565632390, 139.8420026707766226, -13.00000000000000000 ) ) ;
#16651 = CARTESIAN_POINT ( 'NONE',  ( 0.000000000000000000, 242.9999999999997158, 45.00000000000000000 ) ) ;
#16653 = ORIENTED_EDGE ( 'NONE', *, *, #19514, .T. ) ;
#16652 = EDGE_LOOP ( 'NONE', ( #9455, #12357, #19361, #12950 ) ) ;
#16654 = CIRCLE ( 'NONE', #26278, 22.49999999999997868 ) ;
#16655 = CARTESIAN_POINT ( 'NONE',  ( 158.0000000000014495, 68.01962454207041731, -45.00000000000000000 ) ) ;
#16656 = ORIENTED_EDGE ( 'NONE', *, *, #17829, .T. ) ;
#16657 = ORIENTED_EDGE ( 'NONE', *, *, #14017, .T. ) ;
#16658 = EDGE_CURVE ( 'NONE', #2371, #20337, #8521, .T. ) ;
#16659 = EDGE_LOOP ( 'NONE', ( #14672, #10681, #26870, #10896 ) ) ;
#16660 = EDGE_CURVE ( 'NONE', #4740, #7009, #6772, .T. ) ;
#16661 = EDGE_CURVE ( 'NONE', #21378, #22270, #22850, .T. ) ;
#16662 = VERTEX_POINT ( 'NONE', #2898 ) ;
#16663 = ORIENTED_EDGE ( 'NONE', *, *, #5625, .F. ) ;
#16664 = ORIENTED_EDGE ( 'NONE', *, *, #14749, .T. ) ;
#16665 = CIRCLE ( 'NONE', #2897, 64.76834224489934400 ) ;
#16666 = DIRECTION ( 'NONE',  ( -0.000000000000000000, -0.000000000000000000, -1.000000000000000000 ) ) ;
#16667 = VECTOR ( 'NONE', #7398, 1000.000000000000114 ) ;
#16668 = DIRECTION ( 'NONE',  ( 0.8916010070293584056, -0.4528218681382712996, 0.000000000000000000 ) ) ;
#16669 = AXIS2_PLACEMENT_3D ( 'NONE', #13330, #22079, #22934 ) ;
#16670 = CARTESIAN_POINT ( 'NONE',  ( 109.9513937765169516, 257.9883255678629439, -43.25762702467091003 ) ) ;
#16671 = CARTESIAN_POINT ( 'NONE',  ( -13.46517964523875399, 129.5882704147440450, -16.86081371659212991 ) ) ;
#16672 = DIRECTION ( 'NONE',  ( -0.000000000000000000, -0.000000000000000000, 1.000000000000000000 ) ) ;
#16673 = FACE_OUTER_BOUND ( 'NONE', #16422, .T. ) ;
#16674 = LINE ( 'NONE', #14658, #2417 ) ;
#16675 = DIRECTION ( 'NONE',  ( -1.000000000000000000, -2.602085213965211135E-16, 0.000000000000000000 ) ) ;
#16676 = LINE ( 'NONE', #6030, #863 ) ;
#16677 = DIRECTION ( 'NONE',  ( -0.000000000000000000, -1.000000000000000000, -0.000000000000000000 ) ) ;
#16678 = LINE ( 'NONE', #25432, #19835 ) ;
#16679 = ORIENTED_EDGE ( 'NONE', *, *, #18536, .T. ) ;
#16680 = AXIS2_PLACEMENT_3D ( 'NONE', #21140, #16980, #23727 ) ;
#16681 = CARTESIAN_POINT ( 'NONE',  ( -191.4269953611151891, 102.1549118977063699, 32.85580523774468986 ) ) ;
#16682 = EDGE_CURVE ( 'NONE', #7082, #20397, #3167, .T. ) ;
#16683 = AXIS2_PLACEMENT_3D ( 'NONE', #18567, #22455, #16002 ) ;
#16684 = PRODUCT_DEFINITION_SHAPE ( 'NONE', 'NONE',  #28407 ) ;
#16685 = DIRECTION ( 'NONE',  ( -0.2383857661250380344, -0.9711705445023436356, 0.000000000000000000 ) ) ;
#16686 = VERTEX_POINT ( 'NONE', #18413 ) ;
#16687 = DIRECTION ( 'NONE',  ( 0.000000000000000000, 0.9242245927363030855, 0.3818493186865927203 ) ) ;
#16688 = VECTOR ( 'NONE', #22041, 1000.000000000000000 ) ;
#16689 = VERTEX_POINT ( 'NONE', #16268 ) ;
#16690 = EDGE_LOOP ( 'NONE', ( #13999, #17038, #351, #12292 ) ) ;
#16691 = CARTESIAN_POINT ( 'NONE',  ( 94.38583646783938264, 113.6320904521619610, 99.99999999997838529 ) ) ;
#16692 = CARTESIAN_POINT ( 'NONE',  ( 2.016757918737204225, 1.249999999999999556, 7.548718989644206623 ) ) ;
#16693 = EDGE_CURVE ( 'NONE', #5551, #15968, #5046, .T. ) ;
#16694 = ORIENTED_EDGE ( 'NONE', *, *, #21674, .T. ) ;
#16695 = ORIENTED_EDGE ( 'NONE', *, *, #18313, .T. ) ;
#16696 = DIRECTION ( 'NONE',  ( 0.8916010070293384215, 0.4528218681383106015, 0.000000000000000000 ) ) ;
#16697 = EDGE_CURVE ( 'NONE', #27297, #12778, #14675, .T. ) ;
#16698 = LINE ( 'NONE', #1598, #8818 ) ;
#16699 = FACE_OUTER_BOUND ( 'NONE', #11444, .T. ) ;
#16700 = ORIENTED_EDGE ( 'NONE', *, *, #4895, .T. ) ;
#16701 = CARTESIAN_POINT ( 'NONE',  ( 179.9999999999999147, -5.589247009368136787, -100.0000000000000142 ) ) ;
#16702 = ORIENTED_EDGE ( 'NONE', *, *, #17079, .T. ) ;
#16703 = VECTOR ( 'NONE', #8116, 1000.000000000000000 ) ;
#16704 = DIRECTION ( 'NONE',  ( -4.625929269271489858E-16, 2.100614451407711032E-31, -1.000000000000000000 ) ) ;
#16705 = CARTESIAN_POINT ( 'NONE',  ( 158.0000000000012506, 86.08262460212675649, 45.00000000000000000 ) ) ;
#16706 = DIRECTION ( 'NONE',  ( 0.9682458365518510357, -2.433928644932298160E-14, -0.2500000000000128231 ) ) ;
#16707 = DIRECTION ( 'NONE',  ( 0.4528218681383056610, -0.8916010070293409751, 0.000000000000000000 ) ) ;
#16708 = VECTOR ( 'NONE', #12416, 999.9999999999998863 ) ;
#16709 = DIRECTION ( 'NONE',  ( 1.000000000000000000, 1.321694076934710155E-16, -0.000000000000000000 ) ) ;
#16710 = CARTESIAN_POINT ( 'NONE',  ( 119.9999999999999289, 110.0000000000000142, 100.0000000000000142 ) ) ;
#16711 = CARTESIAN_POINT ( 'NONE',  ( 160.9807621135329612, 204.9999999999998863, -151.0000000000000284 ) ) ;
#16712 = ORIENTED_EDGE ( 'NONE', *, *, #19956, .F. ) ;
#16713 = CARTESIAN_POINT ( 'NONE',  ( 65.00000000000000000, -120.0000000000000995, -69.99999999999998579 ) ) ;
#16714 = CARTESIAN_POINT ( 'NONE',  ( 134.9999999999998579, 220.0000000000000284, 84.99999999999995737 ) ) ;
#16715 = LINE ( 'NONE', #27888, #4672 ) ;
#16716 = LINE ( 'NONE', #5082, #22683 ) ;
#16717 = VERTEX_POINT ( 'NONE', #13983 ) ;
#16718 = CARTESIAN_POINT ( 'NONE',  ( 134.9999999999998579, 220.0000000000000284, -90.00000000000002842 ) ) ;
#16719 = VERTEX_POINT ( 'NONE', #18273 ) ;
#16720 = ADVANCED_FACE ( 'NONE', ( #20420 ), #21089, .F. ) ;
#16721 = LINE ( 'NONE', #6215, #10696 ) ;
#16722 = DIRECTION ( 'NONE',  ( 0.9659258262890662028, -0.2588190451025286221, 0.000000000000000000 ) ) ;
#16723 = DIRECTION ( 'NONE',  ( 0.000000000000000000, 0.000000000000000000, 1.000000000000000000 ) ) ;
#16724 = ORIENTED_EDGE ( 'NONE', *, *, #26195, .F. ) ;
#16725 = CARTESIAN_POINT ( 'NONE',  ( 79.99999999999994316, -40.00000000000002842, 70.00000000000001421 ) ) ;
#16726 = DIRECTION ( 'NONE',  ( -0.000000000000000000, -0.000000000000000000, -1.000000000000000000 ) ) ;
#16727 = VERTEX_POINT ( 'NONE', #25020 ) ;
#16728 = VECTOR ( 'NONE', #13534, 1000.000000000000000 ) ;
#16729 = LINE ( 'NONE', #1353, #15241 ) ;
#16730 = CARTESIAN_POINT ( 'NONE',  ( 109.8949283312402088, 257.8851048416491949, 41.33580947111263981 ) ) ;
#16731 = ORIENTED_EDGE ( 'NONE', *, *, #19956, .T. ) ;
#16732 = AXIS2_PLACEMENT_3D ( 'NONE', #6151, #17207, #19782 ) ;
#16733 = VERTEX_POINT ( 'NONE', #3031 ) ;
#16734 = DIRECTION ( 'NONE',  ( 0.000000000000000000, 0.000000000000000000, -1.000000000000000000 ) ) ;
#16735 = ORIENTED_EDGE ( 'NONE', *, *, #23129, .T. ) ;
#16736 = ADVANCED_FACE ( 'NONE', ( #20698 ), #22298, .F. ) ;
#16737 = EDGE_CURVE ( 'NONE', #6433, #24464, #451, .T. ) ;
#16738 = ORIENTED_EDGE ( 'NONE', *, *, #7431, .F. ) ;
#16739 = ORIENTED_EDGE ( 'NONE', *, *, #16533, .F. ) ;
#16740 = DIRECTION ( 'NONE',  ( 0.4528218681382912836, -0.8916010070293483025, 0.000000000000000000 ) ) ;
#16741 = CARTESIAN_POINT ( 'NONE',  ( -210.0000000000000853, -213.8933171992502196, 109.9063181431897505 ) ) ;
#16742 = CARTESIAN_POINT ( 'NONE',  ( -175.8417606860892874, 246.9430296707336652, -15.00000000000000000 ) ) ;
#16743 = VECTOR ( 'NONE', #20236, 1000.000000000000114 ) ;
#16744 = EDGE_CURVE ( 'NONE', #28048, #3815, #7903, .T. ) ;
#16745 = CARTESIAN_POINT ( 'NONE',  ( 115.9275995189148603, 208.0497038390087710, -99.13875753836940419 ) ) ;
#16746 = CARTESIAN_POINT ( 'NONE',  ( 157.4999999999996589, 278.9350626764145318, -45.00000000000000000 ) ) ;
#16747 = CARTESIAN_POINT ( 'NONE',  ( -220.6363270246462776, 61.10744949787153502, -10.70339401868749896 ) ) ;
#16748 = ADVANCED_FACE ( 'NONE', ( #11956 ), #13545, .T. ) ;
#16749 = CARTESIAN_POINT ( 'NONE',  ( -17.24491960465746132, 75.97823757117562593, 100.0000000000000000 ) ) ;
#16750 = AXIS2_PLACEMENT_3D ( 'NONE', #4906, #4473, #11544 ) ;
#16751 = DIRECTION ( 'NONE',  ( -0.6681556583950213346, -0.7440215159218956931, 0.000000000000000000 ) ) ;
#16752 = LINE ( 'NONE', #1232, #23336 ) ;
#16753 = LINE ( 'NONE', #1092, #14852 ) ;
#16754 = ORIENTED_EDGE ( 'NONE', *, *, #17891, .T. ) ;
#16755 = LINE ( 'NONE', #19043, #1763 ) ;
#16756 = DIRECTION ( 'NONE',  ( 0.4528218681371111165, -0.8916010070299477119, 0.000000000000000000 ) ) ;
#16757 = LINE ( 'NONE', #25509, #222 ) ;
#16758 = EDGE_CURVE ( 'NONE', #18364, #9383, #9518, .T. ) ;
#16759 = SURFACE_STYLE_FILL_AREA ( #27651 ) ;
#16760 = DIRECTION ( 'NONE',  ( 0.000000000000000000, 0.000000000000000000, -1.000000000000000000 ) ) ;
#16761 = ORIENTED_EDGE ( 'NONE', *, *, #4624, .T. ) ;
#16762 = CARTESIAN_POINT ( 'NONE',  ( 124.3660254037845192, 199.5814157129575506, 45.00000000000000000 ) ) ;
#16763 = VERTEX_POINT ( 'NONE', #17989 ) ;
#16764 = DIRECTION ( 'NONE',  ( 0.000000000000000000, 0.000000000000000000, -1.000000000000000000 ) ) ;
#16765 = ORIENTED_EDGE ( 'NONE', *, *, #14843, .F. ) ;
#16766 = VECTOR ( 'NONE', #14728, 1000.000000000000000 ) ;
#16767 = VECTOR ( 'NONE', #6702, 999.9999999999998863 ) ;
#16768 = EDGE_LOOP ( 'NONE', ( #10902, #20509, #18332, #9768, #9448, #20564, #20890, #5733, #15731, #10401, #22119, #21102 ) ) ;
#16769 = CARTESIAN_POINT ( 'NONE',  ( -62.44622725233823246, 134.9080593881841139, 13.78052965331430180 ) ) ;
#16770 = VERTEX_POINT ( 'NONE', #2607 ) ;
#16771 = VECTOR ( 'NONE', #15247, 1000.000000000000000 ) ;
#16772 = VERTEX_POINT ( 'NONE', #20282 ) ;
#16773 = DIRECTION ( 'NONE',  ( -0.8916010070293584056, 0.4528218681382713551, 0.000000000000000000 ) ) ;
#16774 = LINE ( 'NONE', #7860, #18700 ) ;
#16775 = PLANE ( 'NONE',  #11147 ) ;
#16776 = CARTESIAN_POINT ( 'NONE',  ( -141.7175972931275680, 126.5060204430971140, -18.19504477830727751 ) ) ;
#16777 = CARTESIAN_POINT ( 'NONE',  ( 157.9999999999996305, 288.7126252026890256, 45.00000000000000000 ) ) ;
#16778 = CARTESIAN_POINT ( 'NONE',  ( 367.4999999999996021, -5.589247009368149222, 1.243177022048955014E-14 ) ) ;
#16779 = CARTESIAN_POINT ( 'NONE',  ( -270.9384205528269831, -170.2669023585998218, 87.94298069144645069 ) ) ;
#16780 = CARTESIAN_POINT ( 'NONE',  ( 167.4999999999996589, 258.6181251126050711, 1.387778780781445676E-14 ) ) ;
#16781 = VECTOR ( 'NONE', #11840, 1000.000000000000000 ) ;
#16782 = CARTESIAN_POINT ( 'NONE',  ( -224.1971796646980408, 86.90724828645529954, 16.84710691662892046 ) ) ;
#16783 = CARTESIAN_POINT ( 'NONE',  ( -221.3650667873343139, -91.18033988749901653, 0.000000000000000000 ) ) ;
#16784 = DIRECTION ( 'NONE',  ( 1.000000000000000000, 0.000000000000000000, -0.000000000000000000 ) ) ;
#16785 = PLANE ( 'NONE',  #26728 ) ;
#16786 = CIRCLE ( 'NONE', #1190, 2.000000000000000000 ) ;
#16787 = ORIENTED_EDGE ( 'NONE', *, *, #20582, .F. ) ;
#16788 = EDGE_CURVE ( 'NONE', #22236, #21431, #7069, .T. ) ;
#16789 = CARTESIAN_POINT ( 'NONE',  ( -45.67245149924918479, -18.36872794415985766, 100.0000000000000142 ) ) ;
#16790 = ADVANCED_FACE ( 'NONE', ( #13835 ), #2748, .F. ) ;
#16791 = CARTESIAN_POINT ( 'NONE',  ( 106.5441062369885117, 210.4993626438576086, -144.6099047286054713 ) ) ;
#16792 = AXIS2_PLACEMENT_3D ( 'NONE', #11642, #1123, #25255 ) ;
#16794 = ORIENTED_EDGE ( 'NONE', *, *, #1814, .F. ) ;
#16793 = ORIENTED_EDGE ( 'NONE', *, *, #12017, .F. ) ;
#16795 = DIRECTION ( 'NONE',  ( 0.4528218681379315713, 0.8916010070295309342, -0.000000000000000000 ) ) ;
#16796 = VERTEX_POINT ( 'NONE', #18553 ) ;
#16797 = ORIENTED_EDGE ( 'NONE', *, *, #21438, .T. ) ;
#16798 = ORIENTED_EDGE ( 'NONE', *, *, #16975, .F. ) ;
#16799 = ORIENTED_EDGE ( 'NONE', *, *, #14791, .F. ) ;
#16800 = VERTEX_POINT ( 'NONE', #9226 ) ;
#16801 = ORIENTED_EDGE ( 'NONE', *, *, #18992, .F. ) ;
#16802 = AXIS2_PLACEMENT_3D ( 'NONE', #26080, #23795, #2090 ) ;
#16803 = CARTESIAN_POINT ( 'NONE',  ( 158.0000000000011937, 93.09837461714084839, 45.00000000000000000 ) ) ;
#16804 = EDGE_CURVE ( 'NONE', #19256, #9167, #22861, .T. ) ;
#16805 = CARTESIAN_POINT ( 'NONE',  ( 157.9999999999998295, 229.0315000300280417, 45.00000000000000000 ) ) ;
#16806 = VECTOR ( 'NONE', #27504, 1000.000000000000000 ) ;
#16807 = CARTESIAN_POINT ( 'NONE',  ( 107.9379936443569221, 247.3367456615697222, -33.97043262446585743 ) ) ;
#16808 = DIRECTION ( 'NONE',  ( -0.000000000000000000, -0.000000000000000000, -1.000000000000000000 ) ) ;
#16809 = DIRECTION ( 'NONE',  ( -0.000000000000000000, -0.000000000000000000, -1.000000000000000000 ) ) ;
#16810 = EDGE_CURVE ( 'NONE', #2468, #22232, #16128, .T. ) ;
#16811 = CARTESIAN_POINT ( 'NONE',  ( 157.4999999999996874, 266.3956876388795649, 45.00000000000000000 ) ) ;
#16812 = CARTESIAN_POINT ( 'NONE',  ( -214.2457779686714900, 55.07866962813993439, -44.91461755630191277 ) ) ;
#16813 = EDGE_CURVE ( 'NONE', #11368, #25971, #16406, .T. ) ;
#16814 = EDGE_CURVE ( 'NONE', #7917, #3880, #4903, .T. ) ;
#16815 = CARTESIAN_POINT ( 'NONE',  ( 112.3311635761228899, 200.3498790610213973, -143.0657854549350816 ) ) ;
#16816 = EDGE_CURVE ( 'NONE', #2018, #23487, #26127, .T. ) ;
#16817 = PLANE ( 'NONE',  #18761 ) ;
#16818 = PLANE ( 'NONE',  #3262 ) ;
#16819 = CARTESIAN_POINT ( 'NONE',  ( -40.40953891503691153, 0.000000000000000000, 99.00000000000000000 ) ) ;
#16820 = VERTEX_POINT ( 'NONE', #3308 ) ;
#16821 = VECTOR ( 'NONE', #18739, 1000.000000000000000 ) ;
#16822 = CARTESIAN_POINT ( 'NONE',  ( -189.6972266830665603, 103.6065584371345949, 32.02885553339256575 ) ) ;
#16823 = DIRECTION ( 'NONE',  ( -0.000000000000000000, -0.000000000000000000, -1.000000000000000000 ) ) ;
#16824 = ORIENTED_EDGE ( 'NONE', *, *, #12670, .F. ) ;
#16825 = CARTESIAN_POINT ( 'NONE',  ( 65.00000000000000000, -114.0000000000000711, 70.00000000000001421 ) ) ;
#16826 = ORIENTED_EDGE ( 'NONE', *, *, #15701, .T. ) ;
#16827 = ORIENTED_EDGE ( 'NONE', *, *, #6489, .F. ) ;
#16828 = CARTESIAN_POINT ( 'NONE',  ( 85.90765579567833754, 110.5723347145563338, 99.99999999998919975 ) ) ;
#16829 = CARTESIAN_POINT ( 'NONE',  ( -203.2481855153402250, 92.57460631283319685, -29.78692811926998729 ) ) ;
#16830 = ORIENTED_EDGE ( 'NONE', *, *, #22149, .T. ) ;
#16831 = ORIENTED_EDGE ( 'NONE', *, *, #14287, .F. ) ;
#16832 = CARTESIAN_POINT ( 'NONE',  ( 158.0000000000001990, 188.3976249024084666, 45.00000000000000000 ) ) ;
#16833 = FACE_OUTER_BOUND ( 'NONE', #25207, .T. ) ;
#16834 = CARTESIAN_POINT ( 'NONE',  ( 158.0000000000009663, 113.6692496847042264, 45.00000000000000000 ) ) ;
#16835 = ORIENTED_EDGE ( 'NONE', *, *, #13101, .T. ) ;
#16836 = CARTESIAN_POINT ( 'NONE',  ( 157.9999999999996874, 271.1575001501400379, 45.00000000000000000 ) ) ;
#16837 = ORIENTED_EDGE ( 'NONE', *, *, #17041, .T. ) ;
#16838 = AXIS2_PLACEMENT_3D ( 'NONE', #3433, #25276, #5598 ) ;
#16839 = ADVANCED_FACE ( 'NONE', ( #27998 ), #23284, .T. ) ;
#16840 = AXIS2_PLACEMENT_3D ( 'NONE', #24541, #9318, #2837 ) ;
#16841 = EDGE_CURVE ( 'NONE', #19335, #6913, #11924, .T. ) ;
#16842 = CARTESIAN_POINT ( 'NONE',  ( 157.9999999999998010, 236.0472500450420341, -45.00000000000000000 ) ) ;
#16843 = CARTESIAN_POINT ( 'NONE',  ( 109.9999999999999289, -90.00000000000001421, -25.00000000000000000 ) ) ;
#16844 = CARTESIAN_POINT ( 'NONE',  ( -33.75989249264057435, 129.4008931478827833, -15.57934110460595001 ) ) ;
#16845 = CARTESIAN_POINT ( 'NONE',  ( 158.0000000000013074, 83.06687458711267880, 45.00000000000000000 ) ) ;
#16846 = DIRECTION ( 'NONE',  ( 1.000000000000000000, 0.000000000000000000, -0.000000000000000000 ) ) ;
#16847 = CARTESIAN_POINT ( 'NONE',  ( -189.5876332061210405, 103.4736392598993717, -32.83942934983755890 ) ) ;
#16848 = ORIENTED_EDGE ( 'NONE', *, *, #26281, .F. ) ;
#16849 = DIRECTION ( 'NONE',  ( -0.000000000000000000, 1.000000000000000000, -0.000000000000000000 ) ) ;
#16850 = EDGE_CURVE ( 'NONE', #10085, #627, #1302, .T. ) ;
#16851 = LINE ( 'NONE', #12135, #27987 ) ;
#16852 = CARTESIAN_POINT ( 'NONE',  ( 157.4999999999998579, 188.6515624061619576, 45.00000000000000000 ) ) ;
#16853 = CARTESIAN_POINT ( 'NONE',  ( 65.00000000000000000, -120.0000000000000995, -69.99999999999998579 ) ) ;
#16854 = VERTEX_POINT ( 'NONE', #14665 ) ;
#16855 = CARTESIAN_POINT ( 'NONE',  ( 147.3660254037842492, 239.4185842870417673, 45.00000000000000000 ) ) ;
#16856 = EDGE_LOOP ( 'NONE', ( #23975, #15867, #9109, #11793 ) ) ;
#16857 = PRODUCT_DEFINITION ( 'UNKNOWN', '', #2838, #560 ) ;
#16858 = CARTESIAN_POINT ( 'NONE',  ( 157.4999999999998579, 58.24206201579573872, 45.00000000000000000 ) ) ;
#16859 = DIRECTION ( 'NONE',  ( -0.2588190451025286221, -0.9659258262890662028, 0.000000000000000000 ) ) ;
#16860 = DIRECTION ( 'NONE',  ( -1.000000000000000000, 0.000000000000000000, 0.000000000000000000 ) ) ;
#16861 = ORIENTED_EDGE ( 'NONE', *, *, #3717, .T. ) ;
#16862 = DIRECTION ( 'NONE',  ( -0.000000000000000000, 1.000000000000000000, -0.000000000000000000 ) ) ;
#16863 = DIRECTION ( 'NONE',  ( 0.000000000000000000, 0.000000000000000000, -1.000000000000000000 ) ) ;
#16864 = EDGE_LOOP ( 'NONE', ( #20314, #16034, #13810, #9028 ) ) ;
#16865 = VECTOR ( 'NONE', #10476, 1000.000000000000000 ) ;
#16866 = CARTESIAN_POINT ( 'NONE',  ( 157.4999999999997726, 243.8248125713165280, -45.00000000000000000 ) ) ;
#16867 = DIRECTION ( 'NONE',  ( 0.7071067811865494601, 0.000000000000000000, 0.7071067811865456854 ) ) ;
#16868 = ORIENTED_EDGE ( 'NONE', *, *, #23404, .F. ) ;
#16869 = ORIENTED_EDGE ( 'NONE', *, *, #16626, .F. ) ;
#16870 = DIRECTION ( 'NONE',  ( 1.000000000000000000, -0.000000000000000000, -0.000000000000000000 ) ) ;
#16871 = ORIENTED_EDGE ( 'NONE', *, *, #514, .F. ) ;
#16872 = ORIENTED_EDGE ( 'NONE', *, *, #24622, .T. ) ;
#16873 = ORIENTED_EDGE ( 'NONE', *, *, #8413, .F. ) ;
#16874 = CARTESIAN_POINT ( 'NONE',  ( -244.5479615644635487, 75.99513337129094737, 5.000000000000002665 ) ) ;
#16875 = AXIS2_PLACEMENT_3D ( 'NONE', #5433, #23249, #25115 ) ;
#16876 = EDGE_CURVE ( 'NONE', #3706, #17245, #1439, .T. ) ;
#16877 = CARTESIAN_POINT ( 'NONE',  ( -180.0000000000000284, 59.99999999999994316, 70.00000000000000000 ) ) ;
#16878 = CARTESIAN_POINT ( 'NONE',  ( -5.301155171372935904, 133.7253830476667247, 14.04417486721310127 ) ) ;
#16879 = CARTESIAN_POINT ( 'NONE',  ( 179.9999999999999147, -5.589247009368136787, -100.0000000000000142 ) ) ;
#16880 = CARTESIAN_POINT ( 'NONE',  ( 119.9999999999999432, 2.220446049250311819E-14, -100.0000000000000142 ) ) ;
#16881 = CARTESIAN_POINT ( 'NONE',  ( -218.4636426211937987, 60.67881959240489920, -11.81164476506858207 ) ) ;
#16882 = FACE_OUTER_BOUND ( 'NONE', #23707, .T. ) ;
#16883 = CARTESIAN_POINT ( 'NONE',  ( 157.4999999999998579, 223.7618125112605298, 45.00000000000000000 ) ) ;
#16884 = DIRECTION ( 'NONE',  ( -9.875160952879181910E-17, 0.000000000000000000, -1.000000000000000000 ) ) ;
#16885 = CARTESIAN_POINT ( 'NONE',  ( 157.9999999999997158, 259.1260001201120531, 45.00000000000000000 ) ) ;
#16886 = ORIENTED_EDGE ( 'NONE', *, *, #24445, .F. ) ;
#16887 = CARTESIAN_POINT ( 'NONE',  ( 3.660298066448477439, -2.383854334960948229, 45.00000000000000000 ) ) ;
#16888 = EDGE_CURVE ( 'NONE', #23507, #17680, #5891, .T. ) ;
#16889 = CIRCLE ( 'NONE', #25144, 30.00000000000000000 ) ;
#16890 = CARTESIAN_POINT ( 'NONE',  ( 2.016757918737201560, -1.250000000000000444, 7.548718989644205735 ) ) ;
#16891 = DIRECTION ( 'NONE',  ( 0.8916010070298049373, -0.4528218681373920584, 0.000000000000000000 ) ) ;
#16892 = CARTESIAN_POINT ( 'NONE',  ( 158.0000000000012790, 83.57474959461971764, 45.00000000000000000 ) ) ;
#16893 = VERTEX_POINT ( 'NONE', #16959 ) ;
#16894 = CONICAL_SURFACE ( 'NONE', #4487, 7.475068018844455153, 0.08726646259971666819 ) ;
#16895 = CARTESIAN_POINT ( 'NONE',  ( 158.0000000000004547, 165.8267498348450886, 45.00000000000000000 ) ) ;
#16896 = ORIENTED_EDGE ( 'NONE', *, *, #24433, .F. ) ;
#16897 = DIRECTION ( 'NONE',  ( 0.8916010070293483025, 0.4528218681382912836, 0.000000000000000000 ) ) ;
#16898 = VECTOR ( 'NONE', #12272, 1000.000000000000000 ) ;
#16899 = ORIENTED_EDGE ( 'NONE', *, *, #2219, .T. ) ;
#16900 =( BOUNDED_SURFACE ( )  B_SPLINE_SURFACE ( 3, 2, ( 
 ( #18048, #2373, #6556 ),
 ( #4527, #6833, #17751 ),
 ( #13180, #20046, #26366 ),
 ( #24223, #15336, #26502 ),
 ( #4670, #4958, #15615 ),
 ( #26806, #20195, #2807 ),
 ( #4817, #24358, #22210 ),
 ( #13316, #22066, #9435 ),
 ( #523, #11599, #11306 ),
 ( #8852, #380, #17611 ),
 ( #19765, #6695, #15908 ),
 ( #15476, #11155, #20339 ),
 ( #13458, #2662, #6973 ),
 ( #2514, #9139, #667 ),
 ( #17900, #2229, #8998 ),
 ( #18197, #90, #239 ),
 ( #24089, #21923, #11014 ),
 ( #26648, #19909, #15763 ),
 ( #24510, #13606, #7128 ),
 ( #22354, #11451, #4395 ),
 ( #9283, #24653, #13748 ),
 ( #22499, #16044, #9710 ),
 ( #14169, #5251, #3226 ),
 ( #1082, #11878, #13896 ),
 ( #27356, #5677, #27492 ),
 ( #7830, #16600, #7695 ),
 ( #20482, #23202, #27222 ),
 ( #12159, #7415, #9573 ),
 ( #807, #21038, #18334 ),
 ( #7563, #5532, #22922 ) ),
 .UNSPECIFIED., .F., .F., .F. ) 
 B_SPLINE_SURFACE_WITH_KNOTS ( ( 4, 2, 2, 2, 2, 2, 2, 2, 2, 2, 2, 2, 2, 2, 4 ),
 ( 3, 3 ),
 ( 0.000000000000000000, 0.003854887539719073237, 0.007709775079438146474, 0.009637218849297683743, 0.01156466261915722014, 0.01541955015887629295, 0.01927443769859536749, 0.02312932523831444029, 0.03083910031775258589, 0.03469398785747165870, 0.03854887539719073497, 0.04625865047662888058, 0.05396842555606702618, 0.05782331309578610246, 0.06167820063550517179 ),
 ( 0.000000000000000000, 1.000000000000000000 ),
 .UNSPECIFIED. ) 
 GEOMETRIC_REPRESENTATION_ITEM ( )  RATIONAL_B_SPLINE_SURFACE ( (
 ( 1.000000000000000000, 0.7071067811865476838, 1.000000000000000000),
 ( 1.000000000000000000, 0.7108376764366090006, 1.000000000000000000),
 ( 1.000000000000000000, 0.7158505121290739126, 1.000000000000000000),
 ( 1.000000000000000000, 0.7278978148820525185, 1.000000000000000000),
 ( 1.000000000000000000, 0.7349313210305764565, 1.000000000000000000),
 ( 1.000000000000000000, 0.7466216138176463568, 1.000000000000000000),
 ( 1.000000000000000000, 0.7507087799370647518, 1.000000000000000000),
 ( 1.000000000000000000, 0.7592063458285337463, 1.000000000000000000),
 ( 1.000000000000000000, 0.7635836989923795448, 1.000000000000000000),
 ( 1.000000000000000000, 0.7769550404246040598, 1.000000000000000000),
 ( 1.000000000000000000, 0.7862062597107043471, 1.000000000000000000),
 ( 1.000000000000000000, 0.8049739164098205224, 1.000000000000000000),
 ( 1.000000000000000000, 0.8144916847796412895, 1.000000000000000000),
 ( 1.000000000000000000, 0.8334855532651173071, 1.000000000000000000),
 ( 1.000000000000000000, 0.8428380035008721238, 1.000000000000000000),
 ( 1.000000000000000000, 0.8700856926953133286, 1.000000000000000000),
 ( 1.000000000000000000, 0.8872021369655685996, 1.000000000000000000),
 ( 1.000000000000000000, 0.9106340391008400648, 1.000000000000000000),
 ( 1.000000000000000000, 0.9180764524646015667, 1.000000000000000000),
 ( 1.000000000000000000, 0.9321377268943903394, 1.000000000000000000),
 ( 1.000000000000000000, 0.9386792981679147330, 1.000000000000000000),
 ( 1.000000000000000000, 0.9568359836586407541, 1.000000000000000000),
 ( 1.000000000000000000, 0.9669855263615203533, 1.000000000000000000),
 ( 1.000000000000000000, 0.9833405099229461932, 1.000000000000000000),
 ( 1.000000000000000000, 0.9895476861110599209, 1.000000000000000000),
 ( 1.000000000000000000, 0.9958061391665089523, 1.000000000000000000),
 ( 1.000000000000000000, 0.9973811977639622794, 1.000000000000000000),
 ( 1.000000000000000000, 0.9994757700715640736, 1.000000000000000000),
 ( 1.000000000000000000, 1.000000000000000000, 1.000000000000000000),
 ( 1.000000000000000000, 1.000000000000000000, 1.000000000000000000) ) ) 
 REPRESENTATION_ITEM ( '' )  SURFACE ( )  );
#16901 = EDGE_CURVE ( 'NONE', #18743, #10961, #15811, .T. ) ;
#16902 = VERTEX_POINT ( 'NONE', #27433 ) ;
#16903 = DIRECTION ( 'NONE',  ( -0.000000000000000000, -0.000000000000000000, -1.000000000000000000 ) ) ;
#16904 = EDGE_CURVE ( 'NONE', #15116, #1795, #25293, .T. ) ;
#16905 = ORIENTED_EDGE ( 'NONE', *, *, #20673, .F. ) ;
#16906 = ORIENTED_EDGE ( 'NONE', *, *, #17610, .T. ) ;
#16907 = LINE ( 'NONE', #27807, #5825 ) ;
#16908 = CARTESIAN_POINT ( 'NONE',  ( -43.02437977270766822, 129.7200458115293031, -16.81627168235288394 ) ) ;
#16909 = CARTESIAN_POINT ( 'NONE',  ( 9.999999999999749534, 90.00000000000001421, 110.0000000000000284 ) ) ;
#16910 = AXIS2_PLACEMENT_3D ( 'NONE', #17983, #7210, #9513 ) ;
#16911 = CARTESIAN_POINT ( 'NONE',  ( -149.1990966351883117, 125.0787559347685658, -18.94696671105487695 ) ) ;
#16912 = CARTESIAN_POINT ( 'NONE',  ( -200.0000000000000284, -91.18033988749901653, 0.000000000000000000 ) ) ;
#16913 = CARTESIAN_POINT ( 'NONE',  ( -229.2498027451139251, 132.0565166830976693, 13.00000000000000000 ) ) ;
#16914 = CARTESIAN_POINT ( 'NONE',  ( -232.7412786160992084, 91.52974244978815932, -14.99999999999999645 ) ) ;
#16915 = PRODUCT_DEFINITION_SHAPE ( 'NONE', 'NONE',  #28410 ) ;
#16916 = CARTESIAN_POINT ( 'NONE',  ( 129.0384544366281716, 249.4018031322194702, -145.7833319456713639 ) ) ;
#16917 = AXIS2_PLACEMENT_3D ( 'NONE', #10309, #25252, #21220 ) ;
#16918 = CARTESIAN_POINT ( 'NONE',  ( -222.0883063321265638, 86.46654056963494384, 17.72095034480506470 ) ) ;
#16919 = CARTESIAN_POINT ( 'NONE',  ( 145.7188177565814158, 467.1080826427131001, -145.0000000000000000 ) ) ;
#16920 = CARTESIAN_POINT ( 'NONE',  ( -156.8436863811589603, 180.7779002010536544, 15.00000000000000000 ) ) ;
#16921 = LINE ( 'NONE', #14775, #13011 ) ;
#16922 = ORIENTED_EDGE ( 'NONE', *, *, #26840, .F. ) ;
#16923 = EDGE_CURVE ( 'NONE', #20027, #4329, #18971, .T. ) ;
#16924 = ADVANCED_FACE ( 'NONE', ( #7911 ), #9018, .T. ) ;
#16925 = CARTESIAN_POINT ( 'NONE',  ( -44.64074837118231187, -18.63255001205507355, 99.96486222153572498 ) ) ;
#16926 = DIRECTION ( 'NONE',  ( 0.05364526231779759985, 0.9985600561963485777, 0.000000000000000000 ) ) ;
#16927 = CARTESIAN_POINT ( 'NONE',  ( 158.0000000000002842, 178.8739998798873216, 45.00000000000000000 ) ) ;
#16929 = ORIENTED_EDGE ( 'NONE', *, *, #21905, .F. ) ;
#16928 = ORIENTED_EDGE ( 'NONE', *, *, #23166, .T. ) ;
#16930 = CIRCLE ( 'NONE', #8210, 49.99999999999998579 ) ;
#16931 = CARTESIAN_POINT ( 'NONE',  ( 107.0062495987152715, 249.1467455478701822, -31.68887795646429240 ) ) ;
#16932 = ORIENTED_EDGE ( 'NONE', *, *, #10979, .T. ) ;
#16933 = VERTEX_POINT ( 'NONE', #15094 ) ;
#16934 = EDGE_CURVE ( 'NONE', #11042, #7588, #147, .T. ) ;
#16935 = ORIENTED_EDGE ( 'NONE', *, *, #18925, .F. ) ;
#16936 = ORIENTED_EDGE ( 'NONE', *, *, #10331, .F. ) ;
#16937 = EDGE_LOOP ( 'NONE', ( #1667, #13031, #12346, #26736 ) ) ;
#16938 = EDGE_LOOP ( 'NONE', ( #16541, #22777, #16831, #17703 ) ) ;
#16939 = EDGE_CURVE ( 'NONE', #13442, #8669, #21974, .T. ) ;
#16940 = CARTESIAN_POINT ( 'NONE',  ( 158.0000000000015916, 53.48024950453520177, 45.00000000000000000 ) ) ;
#16942 = EDGE_CURVE ( 'NONE', #16979, #12184, #1364, .T. ) ;
#16941 = VECTOR ( 'NONE', #1288, 1000.000000000000000 ) ;
#16943 = FACE_OUTER_BOUND ( 'NONE', #23332, .T. ) ;
#16944 = EDGE_CURVE ( 'NONE', #25070, #25446, #12042, .T. ) ;
#16945 = FACE_OUTER_BOUND ( 'NONE', #23288, .T. ) ;
#16946 = DIRECTION ( 'NONE',  ( 1.000000000000000000, 0.000000000000000000, 0.000000000000000000 ) ) ;
#16947 = CONICAL_SURFACE ( 'NONE', #13289, 16.36034929305424512, 0.08885387018394150238 ) ;
#16948 = VECTOR ( 'NONE', #14616, 999.9999999999998863 ) ;
#16949 = CARTESIAN_POINT ( 'NONE',  ( 157.9999999999998579, 219.0000000000000284, 45.00000000000000000 ) ) ;
#16950 = CARTESIAN_POINT ( 'NONE',  ( 187.4999999999996305, -5.589247009368140340, -74.99999999999995737 ) ) ;
#16951 = CARTESIAN_POINT ( 'NONE',  ( -207.5699030661693030, 75.55056756148773900, -43.24289214104831558 ) ) ;
#16952 = VECTOR ( 'NONE', #988, 1000.000000000000000 ) ;
#16953 = CARTESIAN_POINT ( 'NONE',  ( 111.7339150226400619, 201.0596247756230355, -141.3391815462163663 ) ) ;
#16954 = DIRECTION ( 'NONE',  ( -1.000000000000000000, 0.000000000000000000, 0.000000000000000000 ) ) ;
#16955 = EDGE_CURVE ( 'NONE', #25616, #19117, #13954, .T. ) ;
#16956 = CARTESIAN_POINT ( 'NONE',  ( 157.4999999999998579, 138.4940622560211239, 45.00000000000000000 ) ) ;
#16957 = DIRECTION ( 'NONE',  ( -0.000000000000000000, -0.000000000000000000, -1.000000000000000000 ) ) ;
#16958 = VERTEX_POINT ( 'NONE', #11359 ) ;
#16959 = CARTESIAN_POINT ( 'NONE',  ( -42.99650729631200363, 36.92584315232891612, 99.00000000000000000 ) ) ;
#16960 = AXIS2_PLACEMENT_3D ( 'NONE', #11915, #26841, #24972 ) ;
#16961 = DIRECTION ( 'NONE',  ( -3.469446951953614189E-16, 1.000000000000000000, 0.000000000000000000 ) ) ;
#16962 = EDGE_LOOP ( 'NONE', ( #18844, #368, #3942, #399 ) ) ;
#16963 = ORIENTED_EDGE ( 'NONE', *, *, #25902, .T. ) ;
#16964 = VERTEX_POINT ( 'NONE', #17805 ) ;
#16965 = CARTESIAN_POINT ( 'NONE',  ( 154.4185842870420799, 207.6339745962155803, 45.00000000000000000 ) ) ;
#16966 = CIRCLE ( 'NONE', #18373, 6.025000000000002132 ) ;
#16967 = CARTESIAN_POINT ( 'NONE',  ( 158.0000000000001137, 195.9212499249295831, 45.00000000000000000 ) ) ;
#16968 = ORIENTED_EDGE ( 'NONE', *, *, #5394, .T. ) ;
#16969 = EDGE_LOOP ( 'NONE', ( #16296, #19197, #20535, #4419 ) ) ;
#16970 = ADVANCED_FACE ( 'NONE', ( #24564 ), #22264, .F. ) ;
#16971 = CARTESIAN_POINT ( 'NONE',  ( 157.9999999999996589, 279.1890001801680796, 45.00000000000000000 ) ) ;
#16972 = EDGE_CURVE ( 'NONE', #5280, #5095, #4872, .T. ) ;
#16973 = CIRCLE ( 'NONE', #13778, 5.999999999999991118 ) ;
#16974 = CARTESIAN_POINT ( 'NONE',  ( 107.0237601845336712, 245.0637783987590694, 31.95154820714027366 ) ) ;
#16975 = EDGE_CURVE ( 'NONE', #24347, #18723, #17954, .T. ) ;
#16976 = CARTESIAN_POINT ( 'NONE',  ( -189.6091703120771967, 103.6687479389959350, -32.02356223315309336 ) ) ;
#16977 = ORIENTED_EDGE ( 'NONE', *, *, #27785, .T. ) ;
#16978 = CARTESIAN_POINT ( 'NONE',  ( 46.36636626309694975, -15.13258561588589757, 45.00000000000000000 ) ) ;
#16979 = VERTEX_POINT ( 'NONE', #2720 ) ;
#16980 = DIRECTION ( 'NONE',  ( 1.000000000000000000, 0.000000000000000000, 0.000000000000000000 ) ) ;
#16981 = CYLINDRICAL_SURFACE ( 'NONE', #24990, 5.000000000000004441 ) ;
#16982 = CARTESIAN_POINT ( 'NONE',  ( -524.0002167759885197, -169.4627935898112696, 0.000000000000000000 ) ) ;
#16983 = CARTESIAN_POINT ( 'NONE',  ( 163.3555207136468539, 210.2026635890346711, -146.9347961558894156 ) ) ;
#16984 = ORIENTED_EDGE ( 'NONE', *, *, #54, .F. ) ;
#16985 = CIRCLE ( 'NONE', #5528, 2.000000000000000000 ) ;
#16986 = DIRECTION ( 'NONE',  ( -0.000000000000000000, -0.000000000000000000, -1.000000000000000000 ) ) ;
#16987 = LINE ( 'NONE', #6636, #24353 ) ;
#16988 = CARTESIAN_POINT ( 'NONE',  ( 157.4999999999995737, 203.6988124512014338, 45.00000000000000000 ) ) ;
#16989 = DIRECTION ( 'NONE',  ( -0.000000000000000000, -0.000000000000000000, -1.000000000000000000 ) ) ;
#16990 = ORIENTED_EDGE ( 'NONE', *, *, #23570, .F. ) ;
#16991 = DIRECTION ( 'NONE',  ( -0.000000000000000000, -0.000000000000000000, -1.000000000000000000 ) ) ;
#16992 = VECTOR ( 'NONE', #5513, 1000.000000000000114 ) ;
#16993 = LINE ( 'NONE', #17137, #28126 ) ;
#16994 = CARTESIAN_POINT ( 'NONE',  ( -27.13451380343252595, 127.9642796392991784, -17.52013407737619488 ) ) ;
#16995 = CARTESIAN_POINT ( 'NONE',  ( -207.4141359493844732, 90.18508254785665201, 25.67621972994781387 ) ) ;
#16996 = ORIENTED_EDGE ( 'NONE', *, *, #23175, .F. ) ;
#16997 = CARTESIAN_POINT ( 'NONE',  ( 158.0000000000001705, 188.9054999099155054, 45.00000000000000000 ) ) ;
#16998 = ORIENTED_EDGE ( 'NONE', *, *, #13674, .F. ) ;
#16999 = CARTESIAN_POINT ( 'NONE',  ( 132.3894761555988282, 239.8288972274758919, 45.00000000000000000 ) ) ;
#17000 = CARTESIAN_POINT ( 'NONE',  ( 157.4999999999998579, 183.6358123911478799, 45.00000000000000000 ) ) ;
#17001 = ORIENTED_EDGE ( 'NONE', *, *, #3413, .F. ) ;
#17002 = ORIENTED_EDGE ( 'NONE', *, *, #26185, .F. ) ;
#17003 = ADVANCED_FACE ( 'NONE', ( #26561 ), #18246, .T. ) ;
#17004 = CARTESIAN_POINT ( 'NONE',  ( 217.4999999999996305, 258.6181251126050711, 1.387778780781445676E-14 ) ) ;
#17005 = EDGE_LOOP ( 'NONE', ( #28141, #27699, #3393, #19937 ) ) ;
#17006 = VECTOR ( 'NONE', #5576, 1000.000000000000000 ) ;
#17007 = ADVANCED_FACE ( 'NONE', ( #9343 ), #9627, .F. ) ;
#17008 = VERTEX_POINT ( 'NONE', #20248 ) ;
#17009 = ORIENTED_EDGE ( 'NONE', *, *, #3832, .T. ) ;
#17010 = CARTESIAN_POINT ( 'NONE',  ( -277.2150368962633706, -237.2150368962634559, 110.0000000000000142 ) ) ;
#17011 = VECTOR ( 'NONE', #19426, 1000.000000000000000 ) ;
#17012 = CARTESIAN_POINT ( 'NONE',  ( -210.0000000000000568, -210.8114316696540982, 110.0000000000000284 ) ) ;
#17013 = PLANE ( 'NONE',  #15796 ) ;
#17014 = FACE_OUTER_BOUND ( 'NONE', #19516, .T. ) ;
#17015 = CARTESIAN_POINT ( 'NONE',  ( -76.25760768171835480, 221.6666220619076739, -13.00000000000000000 ) ) ;
#17016 = DIRECTION ( 'NONE',  ( 1.000000000000000000, -0.000000000000000000, -0.000000000000000000 ) ) ;
#17017 = CARTESIAN_POINT ( 'NONE',  ( -220.5365384948384531, 71.33200643683619546, -21.30906822952401924 ) ) ;
#17018 = ORIENTED_EDGE ( 'NONE', *, *, #8675, .F. ) ;
#17019 = DIRECTION ( 'NONE',  ( 0.000000000000000000, -1.000000000000000000, 0.000000000000000000 ) ) ;
#17020 = VECTOR ( 'NONE', #5027, 1000.000000000000000 ) ;
#17021 = CARTESIAN_POINT ( 'NONE',  ( 157.4999999999998579, 110.9074371734436255, 45.00000000000000000 ) ) ;
#17022 = CARTESIAN_POINT ( 'NONE',  ( 157.4999999999998579, 45.70268697826052318, 45.00000000000000000 ) ) ;
#17023 = CARTESIAN_POINT ( 'NONE',  ( 112.6399768800336005, 217.4434959555082116, -96.77053691278551639 ) ) ;
#17024 = ORIENTED_EDGE ( 'NONE', *, *, #18181, .T. ) ;
#17025 = DIRECTION ( 'NONE',  ( -0.000000000000000000, -0.000000000000000000, -1.000000000000000000 ) ) ;
#17026 = CIRCLE ( 'NONE', #14296, 2.000000000000012879 ) ;
#17027 = LINE ( 'NONE', #20815, #27636 ) ;
#17028 = CARTESIAN_POINT ( 'NONE',  ( 282.4999999999996589, 19.41075299063184900, 95.49671038392668265 ) ) ;
#17029 = DIRECTION ( 'NONE',  ( 4.540956701092242152E-16, 1.000000000000000000, 0.000000000000000000 ) ) ;
#17030 = CARTESIAN_POINT ( 'NONE',  ( -210.0000000000001137, -157.0000000000000284, 105.0000000000000284 ) ) ;
#17031 = CARTESIAN_POINT ( 'NONE',  ( -140.1240808061633345, 61.15703788601678781, -145.0000000000000000 ) ) ;
#17032 = ORIENTED_EDGE ( 'NONE', *, *, #26982, .T. ) ;
#17033 = CIRCLE ( 'NONE', #20231, 30.00000000000000000 ) ;
#17034 = EDGE_CURVE ( 'NONE', #20037, #11369, #4107, .T. ) ;
#17035 = CARTESIAN_POINT ( 'NONE',  ( 157.9999999999996305, 286.2047501951820436, 45.00000000000000000 ) ) ;
#17036 = VERTEX_POINT ( 'NONE', #22554 ) ;
#17037 = FACE_OUTER_BOUND ( 'NONE', #11832, .T. ) ;
#17038 = ORIENTED_EDGE ( 'NONE', *, *, #21618, .F. ) ;
#17039 = EDGE_LOOP ( 'NONE', ( #11080, #9123, #2735, #15358, #22808, #12948 ) ) ;
#17040 = CARTESIAN_POINT ( 'NONE',  ( -86.54628362417027176, 136.4599498150971613, 13.48322064102051776 ) ) ;
#17041 = EDGE_CURVE ( 'NONE', #14477, #4345, #18386, .T. ) ;
#17042 = VERTEX_POINT ( 'NONE', #4729 ) ;
#17043 = ORIENTED_EDGE ( 'NONE', *, *, #21926, .F. ) ;
#17044 = PLANE ( 'NONE',  #6745 ) ;
#17045 = CARTESIAN_POINT ( 'NONE',  ( -141.5841712291289127, 126.5472752318202936, -18.17431859372913294 ) ) ;
#17046 = DIRECTION ( 'NONE',  ( -0.000000000000000000, -0.000000000000000000, -1.000000000000000000 ) ) ;
#17047 = ADVANCED_FACE ( 'NONE', ( #8717 ), #93, .F. ) ;
#17048 = VECTOR ( 'NONE', #6245, 1000.000000000000000 ) ;
#17049 = CARTESIAN_POINT ( 'NONE',  ( -112.9218146637504674, 134.5565441768181074, -15.44239355050386564 ) ) ;
#17050 = VECTOR ( 'NONE', #475, 999.9999999999998863 ) ;
#17051 = CIRCLE ( 'NONE', #11087, 67.21503689626328537 ) ;
#17052 = VECTOR ( 'NONE', #14221, 1000.000000000000000 ) ;
#17053 = DIRECTION ( 'NONE',  ( -0.000000000000000000, -0.000000000000000000, -1.000000000000000000 ) ) ;
#17054 = CARTESIAN_POINT ( 'NONE',  ( -66.57029700917655646, 102.2156118568357783, 45.00000000000000000 ) ) ;
#17055 = CARTESIAN_POINT ( 'NONE',  ( -216.2998406815053443, 86.35807036193234865, -20.83938377197658198 ) ) ;
#17056 = CARTESIAN_POINT ( 'NONE',  ( 133.4364168238970194, 249.9598208048105903, -150.7960377432352175 ) ) ;
#17057 = LINE ( 'NONE', #25814, #5738 ) ;
#17058 = DIRECTION ( 'NONE',  ( 1.000000000000000000, -0.000000000000000000, -0.000000000000000000 ) ) ;
#17059 = CARTESIAN_POINT ( 'NONE',  ( 158.0000000000012790, 85.57474959461971764, -45.00000000000000000 ) ) ;
#17060 = VERTEX_POINT ( 'NONE', #20049 ) ;
#17061 = EDGE_CURVE ( 'NONE', #12718, #9667, #17753, .T. ) ;
#17062 = CYLINDRICAL_SURFACE ( 'NONE', #22453, 41.00000000000000711 ) ;
#17063 = LINE ( 'NONE', #107, #15824 ) ;
#17064 = CARTESIAN_POINT ( 'NONE',  ( 157.4999999999998579, 168.5885623461056184, 45.00000000000000000 ) ) ;
#17066 = ORIENTED_EDGE ( 'NONE', *, *, #17238, .F. ) ;
#17065 = ORIENTED_EDGE ( 'NONE', *, *, #4352, .F. ) ;
#17067 = EDGE_CURVE ( 'NONE', #26118, #17211, #10532, .T. ) ;
#17068 = AXIS2_PLACEMENT_3D ( 'NONE', #1197, #22620, #18583 ) ;
#17069 = CARTESIAN_POINT ( 'NONE',  ( 87.50000000000029843, 230.0000000000000000, -15.95262490344447137 ) ) ;
#17070 = ORIENTED_EDGE ( 'NONE', *, *, #18399, .F. ) ;
#17071 = ORIENTED_EDGE ( 'NONE', *, *, #8675, .T. ) ;
#17072 = AXIS2_PLACEMENT_3D ( 'NONE', #13238, #17528, #24427 ) ;
#17073 = VERTEX_POINT ( 'NONE', #24225 ) ;
#17074 = VECTOR ( 'NONE', #23223, 1000.000000000000000 ) ;
#17075 = VERTEX_POINT ( 'NONE', #13461 ) ;
#17076 = ORIENTED_EDGE ( 'NONE', *, *, #15799, .F. ) ;
#17077 = EDGE_LOOP ( 'NONE', ( #17550, #15069, #2451, #22812 ) ) ;
#17078 = CARTESIAN_POINT ( 'NONE',  ( -210.7172313291012529, 103.7585653882801182, 15.00000000000000000 ) ) ;
#17079 = EDGE_CURVE ( 'NONE', #27477, #10183, #20166, .T. ) ;
#17080 = ADVANCED_FACE ( 'NONE', ( #26369 ), #4397, .F. ) ;
#17081 = DIRECTION ( 'NONE',  ( 0.000000000000000000, 0.000000000000000000, 1.000000000000000000 ) ) ;
#17082 = LINE ( 'NONE', #12233, #24951 ) ;
#17083 = VECTOR ( 'NONE', #18228, 1000.000000000000000 ) ;
#17084 = DIRECTION ( 'NONE',  ( 0.000000000000000000, 0.000000000000000000, 1.000000000000000000 ) ) ;
#17085 = AXIS2_PLACEMENT_3D ( 'NONE', #24739, #5330, #26739 ) ;
#17086 = LINE ( 'NONE', #17227, #18586 ) ;
#17087 = AXIS2_PLACEMENT_3D ( 'NONE', #22401, #1126, #25538 ) ;
#17088 = DIRECTION ( 'NONE',  ( -0.8916010070293485246, -0.4528218681382906730, 0.000000000000000000 ) ) ;
#17089 = CARTESIAN_POINT ( 'NONE',  ( 141.9187638636471434, 198.0425250404537678, 45.00000000000000000 ) ) ;
#17090 = EDGE_CURVE ( 'NONE', #5655, #8321, #26505, .T. ) ;
#17091 =( GEOMETRIC_REPRESENTATION_CONTEXT ( 3 ) GLOBAL_UNCERTAINTY_ASSIGNED_CONTEXT ( ( #2554 ) ) GLOBAL_UNIT_ASSIGNED_CONTEXT ( ( #11582, #11861, #4942 ) ) REPRESENTATION_CONTEXT ( 'NONE', 'WORKASPACE' ) );
#17092 = ADVANCED_FACE ( 'NONE', ( #8579 ), #17330, .F. ) ;
#17093 = CYLINDRICAL_SURFACE ( 'NONE', #18290, 5.000000000000004441 ) ;
#17094 = VECTOR ( 'NONE', #22615, 1000.000000000000000 ) ;
#17095 = DIRECTION ( 'NONE',  ( 0.000000000000000000, -1.000000000000000000, 0.000000000000000000 ) ) ;
#17096 = DIRECTION ( 'NONE',  ( 0.000000000000000000, 1.214306433183764966E-16, -1.000000000000000000 ) ) ;
#17097 = DIRECTION ( 'NONE',  ( 0.000000000000000000, 0.000000000000000000, -1.000000000000000000 ) ) ;
#17098 = VERTEX_POINT ( 'NONE', #19767 ) ;
#17099 = CARTESIAN_POINT ( 'NONE',  ( -231.2228484428727882, 90.30500068246439582, -15.11033134556762114 ) ) ;
#17100 = ADVANCED_FACE ( 'NONE', ( #8856 ), #16947, .T. ) ;
#17101 = CARTESIAN_POINT ( 'NONE',  ( -264.1793819498149674, -171.2044657688920211, -109.9235875798455027 ) ) ;
#17102 = EDGE_LOOP ( 'NONE', ( #23928, #16583, #18036, #1068 ) ) ;
#17103 = APPLICATION_PROTOCOL_DEFINITION ( 'draft international standard', 'automotive_design', 1998, #2117 ) ;
#17104 = EDGE_CURVE ( 'NONE', #7444, #27055, #15479, .T. ) ;
#17105 = EDGE_LOOP ( 'NONE', ( #8463, #18833, #17218, #3472 ) ) ;
#17106 = VECTOR ( 'NONE', #5638, 1000.000000000000000 ) ;
#17107 = ORIENTED_EDGE ( 'NONE', *, *, #4414, .F. ) ;
#17108 = AXIS2_PLACEMENT_3D ( 'NONE', #22973, #25927, #26067 ) ;
#17109 = CARTESIAN_POINT ( 'NONE',  ( 90.17595424780135716, 111.7661400906778937, 100.0000000000108429 ) ) ;
#17110 = CARTESIAN_POINT ( 'NONE',  ( 157.9999999999997158, 256.6181251126050711, 45.00000000000000000 ) ) ;
#17111 = ORIENTED_EDGE ( 'NONE', *, *, #2155, .T. ) ;
#17112 = VECTOR ( 'NONE', #22367, 999.9999999999998863 ) ;
#17113 = ORIENTED_EDGE ( 'NONE', *, *, #4957, .F. ) ;
#17114 = CARTESIAN_POINT ( 'NONE',  ( 88.58553289618420479, 111.2425746093144880, -99.99999999998921396 ) ) ;
#17115 = VECTOR ( 'NONE', #26966, 1000.000000000000000 ) ;
#17116 = CARTESIAN_POINT ( 'NONE',  ( 104.2818955975975541, 239.9330879431699657, 27.31284324272755271 ) ) ;
#17117 = CARTESIAN_POINT ( 'NONE',  ( 179.9999999999999147, 526.4263741777961059, -84.99999999999997158 ) ) ;
#17118 = EDGE_LOOP ( 'NONE', ( #15332, #7404, #23653, #17018, #6343, #5971 ) ) ;
#17119 = CARTESIAN_POINT ( 'NONE',  ( -225.0771096875090223, 87.16154696420846903, 16.52804872244989198 ) ) ;
#17120 = EDGE_LOOP ( 'NONE', ( #10054, #11629 ) ) ;
#17121 = FACE_OUTER_BOUND ( 'NONE', #408, .T. ) ;
#17122 = DIRECTION ( 'NONE',  ( 1.000000000000000000, 0.000000000000000000, -0.000000000000000000 ) ) ;
#17123 = DIRECTION ( 'NONE',  ( 0.000000000000000000, -1.000000000000000000, 0.000000000000000000 ) ) ;
#17124 = VECTOR ( 'NONE', #25138, 1000.000000000000000 ) ;
#17125 = CARTESIAN_POINT ( 'NONE',  ( -260.0000000000001137, -167.0819201924624906, -89.99999999999985789 ) ) ;
#17126 = ORIENTED_EDGE ( 'NONE', *, *, #4585, .T. ) ;
#17127 = AXIS2_PLACEMENT_3D ( 'NONE', #21585, #3629, #21301 ) ;
#17128 = DIRECTION ( 'NONE',  ( 0.8916010070296327417, -0.4528218681377311761, 0.000000000000000000 ) ) ;
#17129 = CARTESIAN_POINT ( 'NONE',  ( 184.7759657584203694, 39.02219989801907474, 45.00000000000000000 ) ) ;
#17130 = FACE_OUTER_BOUND ( 'NONE', #27960, .T. ) ;
#17131 = VECTOR ( 'NONE', #8590, 1000.000000000000114 ) ;
#17132 = ADVANCED_FACE ( 'NONE', ( #10874 ), #26087, .F. ) ;
#17133 = FACE_OUTER_BOUND ( 'NONE', #25543, .T. ) ;
#17134 = ORIENTED_EDGE ( 'NONE', *, *, #5146, .T. ) ;
#17135 = CARTESIAN_POINT ( 'NONE',  ( 187.4999999999996305, 258.6181251126050711, 6.000000000000019540 ) ) ;
#17136 = EDGE_CURVE ( 'NONE', #13809, #18951, #24091, .T. ) ;
#17137 = CARTESIAN_POINT ( 'NONE',  ( 158.0000000000013642, 76.05112457209858690, 45.00000000000000000 ) ) ;
#17138 = DIRECTION ( 'NONE',  ( 0.000000000000000000, 0.000000000000000000, 1.000000000000000000 ) ) ;
#17139 = DIRECTION ( 'NONE',  ( -0.000000000000000000, 0.000000000000000000, 1.000000000000000000 ) ) ;
#17140 = EDGE_LOOP ( 'NONE', ( #14187, #3957, #8658, #10268 ) ) ;
#17141 = LINE ( 'NONE', #21165, #28093 ) ;
#17142 = EDGE_LOOP ( 'NONE', ( #66, #28390, #11208, #6674 ) ) ;
#17143 = CARTESIAN_POINT ( 'NONE',  ( 65.00000000000000000, -120.0000000000000995, -76.02499999999999147 ) ) ;
#17144 = CARTESIAN_POINT ( 'NONE',  ( -169.9564382400993168, 115.7522936420806445, -25.38211417480260579 ) ) ;
#17145 = VERTEX_POINT ( 'NONE', #13182 ) ;
#17146 = AXIS2_PLACEMENT_3D ( 'NONE', #26977, #704, #9474 ) ;
#17147 = ORIENTED_EDGE ( 'NONE', *, *, #804, .T. ) ;
#17148 = CARTESIAN_POINT ( 'NONE',  ( -112.3709231662415675, 70.58802258329811252, 82.86315325844958579 ) ) ;
#17149 = ORIENTED_EDGE ( 'NONE', *, *, #14492, .F. ) ;
#17150 = VERTEX_POINT ( 'NONE', #17903 ) ;
#17151 = VERTEX_POINT ( 'NONE', #15193 ) ;
#17152 = AXIS2_PLACEMENT_3D ( 'NONE', #26782, #6949, #499 ) ;
#17153 = LINE ( 'NONE', #15152, #4711 ) ;
#17154 = EDGE_CURVE ( 'NONE', #855, #19117, #9144, .T. ) ;
#17155 = CARTESIAN_POINT ( 'NONE',  ( -205.7061355896892678, 146.0477147645463845, -15.00000000000000000 ) ) ;
#17156 = CARTESIAN_POINT ( 'NONE',  ( 187.4999999999996305, 288.9665627064425166, 45.00000000000000000 ) ) ;
#17157 = CARTESIAN_POINT ( 'NONE',  ( 158.0000000000005116, 160.8109998198309825, 45.00000000000000000 ) ) ;
#17158 = LINE ( 'NONE', #16879, #20210 ) ;
#17159 = LINE ( 'NONE', #19034, #26872 ) ;
#17160 = CARTESIAN_POINT ( 'NONE',  ( -233.3699482038443023, 66.30323757541319196, -6.318463073149253262 ) ) ;
#17161 = ORIENTED_EDGE ( 'NONE', *, *, #2234, .T. ) ;
#17162 = DIRECTION ( 'NONE',  ( 0.000000000000000000, 0.000000000000000000, -1.000000000000000000 ) ) ;
#17163 = ADVANCED_FACE ( 'NONE', ( #13320 ), #22070, .F. ) ;
#17164 = CARTESIAN_POINT ( 'NONE',  ( -216.4421519707229891, 141.6000904446840707, -13.00000000000000000 ) ) ;
#17165 = CARTESIAN_POINT ( 'NONE',  ( 134.9999999999998579, 455.5353319318992362, -145.0000000000000000 ) ) ;
#17166 = CARTESIAN_POINT ( 'NONE',  ( 113.0497540245546304, 214.9557400730136578, -97.19889357486846393 ) ) ;
#17167 = VERTEX_POINT ( 'NONE', #2516 ) ;
#17168 = VECTOR ( 'NONE', #3478, 1000.000000000000000 ) ;
#17169 = ADVANCED_FACE ( 'NONE', ( #11309 ), #23805, .F. ) ;
#17170 = CARTESIAN_POINT ( 'NONE',  ( 157.4999999999998579, 171.0964373536126573, 45.00000000000000000 ) ) ;
#17171 = ADVANCED_FACE ( 'NONE', ( #10738 ), #22357, .T. ) ;
#17172 = EDGE_CURVE ( 'NONE', #16820, #18456, #13311, .T. ) ;
#17173 = DIRECTION ( 'NONE',  ( 1.000000000000000000, -0.000000000000000000, -0.000000000000000000 ) ) ;
#17174 = DIRECTION ( 'NONE',  ( -0.8660254037844394848, 0.4999999999999985012, 0.000000000000000000 ) ) ;
#17175 = CARTESIAN_POINT ( 'NONE',  ( 349.0018770490532916, 96.44595867864244099, -155.7188177565815863 ) ) ;
#17176 = LINE ( 'NONE', #6680, #27141 ) ;
#17177 = DIRECTION ( 'NONE',  ( 0.8660254037844432595, 0.4999999999999919509, -0.000000000000000000 ) ) ;
#17178 = VECTOR ( 'NONE', #13833, 1000.000000000000114 ) ;
#17179 = ORIENTED_EDGE ( 'NONE', *, *, #20845, .F. ) ;
#17180 = FACE_OUTER_BOUND ( 'NONE', #19306, .T. ) ;
#17181 = VERTEX_POINT ( 'NONE', #1085 ) ;
#17182 = DIRECTION ( 'NONE',  ( 0.000000000000000000, 0.000000000000000000, 1.000000000000000000 ) ) ;
#17183 = ORIENTED_EDGE ( 'NONE', *, *, #27848, .F. ) ;
#17184 = VERTEX_POINT ( 'NONE', #20341 ) ;
#17185 = CARTESIAN_POINT ( 'NONE',  ( -210.0000000000000568, -210.8114316696540982, -110.0000000000000284 ) ) ;
#17186 = ORIENTED_EDGE ( 'NONE', *, *, #10526, .T. ) ;
#17187 = ORIENTED_EDGE ( 'NONE', *, *, #19088, .T. ) ;
#17188 = DIRECTION ( 'NONE',  ( 0.000000000000000000, -1.000000000000000000, 0.000000000000000000 ) ) ;
#17189 = VECTOR ( 'NONE', #13501, 999.9999999999998863 ) ;
#17190 = CARTESIAN_POINT ( 'NONE',  ( -77.57255112795054686, 134.6586583231760130, -15.47697172941245469 ) ) ;
#17191 = LINE ( 'NONE', #26085, #127 ) ;
#17192 = CARTESIAN_POINT ( 'NONE',  ( -156.0897298158335786, 122.3430908625673794, -20.70325525780628695 ) ) ;
#17193 = CIRCLE ( 'NONE', #8929, 7.500000000000007105 ) ;
#17194 = EDGE_CURVE ( 'NONE', #10216, #13911, #18889, .T. ) ;
#17195 = CARTESIAN_POINT ( 'NONE',  ( 158.0000000000007674, 131.2243747372535267, -45.00000000000000000 ) ) ;
#17196 = EDGE_CURVE ( 'NONE', #15348, #7126, #9642, .T. ) ;
#17197 = LINE ( 'NONE', #10741, #27772 ) ;
#17198 = CARTESIAN_POINT ( 'NONE',  ( -222.5626178033668623, 88.43593056344644765, -17.20029664898224198 ) ) ;
#17199 = CARTESIAN_POINT ( 'NONE',  ( 129.7957637945470708, 249.5459717953527274, -141.9885977063033522 ) ) ;
#17200 = DIRECTION ( 'NONE',  ( 0.000000000000000000, 0.000000000000000000, -1.000000000000000000 ) ) ;
#17201 = FACE_BOUND ( 'NONE', #8084, .T. ) ;
#17202 = FACE_OUTER_BOUND ( 'NONE', #10808, .T. ) ;
#17203 = CARTESIAN_POINT ( 'NONE',  ( -160.0000000000000284, 59.99999999999994316, -100.0000000000000142 ) ) ;
#17204 = ORIENTED_EDGE ( 'NONE', *, *, #19199, .F. ) ;
#17205 = EDGE_CURVE ( 'NONE', #15878, #23120, #25080, .T. ) ;
#17206 = DIRECTION ( 'NONE',  ( -0.4918581970360879074, 0.000000000000000000, -0.8706753206611571594 ) ) ;
#17207 = DIRECTION ( 'NONE',  ( 0.000000000000000000, -1.000000000000000000, 0.000000000000000000 ) ) ;
#17208 = TOROIDAL_SURFACE ( 'NONE', #11712, 60.90601976618767566, 2.000000000000000000 ) ;
#17209 = DIRECTION ( 'NONE',  ( 1.000000000000000000, -0.000000000000000000, -0.000000000000000000 ) ) ;
#17211 = VERTEX_POINT ( 'NONE', #9438 ) ;
#17210 = ORIENTED_EDGE ( 'NONE', *, *, #7519, .F. ) ;
#17212 = CIRCLE ( 'NONE', #18121, 75.00000000000002842 ) ;
#17213 = CARTESIAN_POINT ( 'NONE',  ( 90.45806322832901003, 239.6644751351067271, -16.82109631826974905 ) ) ;
#17214 = ORIENTED_EDGE ( 'NONE', *, *, #16942, .T. ) ;
#17215 = ORIENTED_EDGE ( 'NONE', *, *, #20537, .T. ) ;
#17216 = AXIS2_PLACEMENT_3D ( 'NONE', #21338, #2938, #7256 ) ;
#17217 = VERTEX_POINT ( 'NONE', #12016 ) ;
#17218 = ORIENTED_EDGE ( 'NONE', *, *, #12897, .F. ) ;
#17219 = ORIENTED_EDGE ( 'NONE', *, *, #5982, .F. ) ;
#17220 = ORIENTED_EDGE ( 'NONE', *, *, #19066, .F. ) ;
#17221 = DIRECTION ( 'NONE',  ( -0.000000000000000000, -0.000000000000000000, -1.000000000000000000 ) ) ;
#17222 = CARTESIAN_POINT ( 'NONE',  ( 157.4999999999998579, 223.7618125112605298, -45.00000000000000000 ) ) ;
#17223 = VECTOR ( 'NONE', #20487, 1000.000000000000000 ) ;
#17224 = VECTOR ( 'NONE', #23955, 1000.000000000000000 ) ;
#17225 = LINE ( 'NONE', #6450, #2776 ) ;
#17226 = ADVANCED_FACE ( 'NONE', ( #18475 ), #26650, .F. ) ;
#17227 = CARTESIAN_POINT ( 'NONE',  ( 158.0000000000007958, 128.7164997297464595, 45.00000000000000000 ) ) ;
#17228 = CIRCLE ( 'NONE', #8527, 7.999999999999979572 ) ;
#17229 = B_SPLINE_CURVE_WITH_KNOTS ( 'NONE', 3,
 ( #21504, #1821, #10596, #23107, #1263, #28100, #16506, #14349, #17623, #15344, #19918, #4680 ),
 .UNSPECIFIED., .F., .F.,
 ( 4, 2, 2, 2, 2, 4 ),
 ( 0.000000000000000000, 0.004258390697697790085, 0.006387586046546603162, 0.008516781395395417106, 0.01277517209309319245, 0.01703356279079096952 ),
 .UNSPECIFIED. ) ;
#17230 = DIRECTION ( 'NONE',  ( 1.000000000000000000, 0.000000000000000000, 0.000000000000000000 ) ) ;
#17231 = CARTESIAN_POINT ( 'NONE',  ( -232.2321867067640824, 76.70661131974999591, -15.57447242055394199 ) ) ;
#17232 = CARTESIAN_POINT ( 'NONE',  ( -27.00790996259407706, 129.1643630886944720, 15.68707935331008940 ) ) ;
#17233 = CARTESIAN_POINT ( 'NONE',  ( -209.4684267455243116, 67.32361167506066124, 34.40574903147302877 ) ) ;
#17234 = FACE_OUTER_BOUND ( 'NONE', #25236, .T. ) ;
#17235 = CARTESIAN_POINT ( 'NONE',  ( -76.25760768171836901, 154.8982798170083299, 12.99999999999999822 ) ) ;
#17236 = EDGE_LOOP ( 'NONE', ( #11654, #8456, #7747, #13583 ) ) ;
#17237 = CARTESIAN_POINT ( 'NONE',  ( -177.9077837340308008, 111.2757406836244627, 29.50435359264835000 ) ) ;
#17238 = EDGE_CURVE ( 'NONE', #26259, #14934, #15767, .T. ) ;
#17239 = EDGE_CURVE ( 'NONE', #2614, #12013, #16966, .T. ) ;
#17240 = CARTESIAN_POINT ( 'NONE',  ( -267.2062018704829143, -170.6788222641287120, -109.5782777413358389 ) ) ;
#17241 = ORIENTED_EDGE ( 'NONE', *, *, #12644, .F. ) ;
#17242 = AXIS2_PLACEMENT_3D ( 'NONE', #130, #10911, #9040 ) ;
#17243 = ORIENTED_EDGE ( 'NONE', *, *, #15722, .T. ) ;
#17244 = AXIS2_PLACEMENT_3D ( 'NONE', #22488, #369, #2653 ) ;
#17245 = VERTEX_POINT ( 'NONE', #22925 ) ;
#17246 = DIRECTION ( 'NONE',  ( 0.8916010070293783896, 0.4528218681382319422, 0.000000000000000000 ) ) ;
#17247 = DIRECTION ( 'NONE',  ( 1.000000000000000000, 0.000000000000000000, -0.000000000000000000 ) ) ;
#17248 = ORIENTED_EDGE ( 'NONE', *, *, #19529, .T. ) ;
#17249 = VECTOR ( 'NONE', #3411, 1000.000000000000000 ) ;
#17251 = EDGE_CURVE ( 'NONE', #4042, #13806, #22504, .T. ) ;
#17250 = ORIENTED_EDGE ( 'NONE', *, *, #24154, .T. ) ;
#17252 = CARTESIAN_POINT ( 'NONE',  ( 114.5273445118729541, 107.2595481030940761, -100.0000000000000142 ) ) ;
#17253 = EDGE_CURVE ( 'NONE', #12700, #19742, #18338, .T. ) ;
#17254 = DIRECTION ( 'NONE',  ( 0.8916010070295005141, -0.4528218681379915789, 0.000000000000000000 ) ) ;
#17255 = DIRECTION ( 'NONE',  ( 0.000000000000000000, -1.000000000000000000, 0.000000000000000000 ) ) ;
#17256 = ORIENTED_EDGE ( 'NONE', *, *, #11713, .F. ) ;
#17257 = CARTESIAN_POINT ( 'NONE',  ( -218.9526947977414579, 86.19408851467024135, 19.27252192978178513 ) ) ;
#17258 = ORIENTED_EDGE ( 'NONE', *, *, #25574, .F. ) ;
#17259 = CARTESIAN_POINT ( 'NONE',  ( -175.0000000000000000, -120.0000000000001847, -69.99999999999998579 ) ) ;
#17260 = CARTESIAN_POINT ( 'NONE',  ( 157.4999999999998579, 220.0000000000000284, -100.0000000000000142 ) ) ;
#17261 = CARTESIAN_POINT ( 'NONE',  ( -115.3221550338875971, 71.54464929955099706, 82.80879831960034210 ) ) ;
#17262 = CIRCLE ( 'NONE', #9473, 5.000000000000000888 ) ;
#17263 = DIRECTION ( 'NONE',  ( -0.000000000000000000, -0.000000000000000000, -1.000000000000000000 ) ) ;
#17264 = ORIENTED_EDGE ( 'NONE', *, *, #3963, .F. ) ;
#17265 = CARTESIAN_POINT ( 'NONE',  ( 157.4999999999998579, 113.4153121809506786, -45.00000000000000000 ) ) ;
#17267 = CARTESIAN_POINT ( 'NONE',  ( 157.4999999999996305, 286.4586876989355915, -45.00000000000000000 ) ) ;
#17266 = VECTOR ( 'NONE', #2203, 1000.000000000000227 ) ;
#17268 = DIRECTION ( 'NONE',  ( 0.4999999999999985012, 0.8660254037844394848, 0.000000000000000000 ) ) ;
#17269 = CARTESIAN_POINT ( 'NONE',  ( 157.4999999999998579, 115.9231871884577174, 45.00000000000000000 ) ) ;
#17270 = ORIENTED_EDGE ( 'NONE', *, *, #18850, .F. ) ;
#17271 = DIRECTION ( 'NONE',  ( 0.000000000000000000, 0.000000000000000000, 1.000000000000000000 ) ) ;
#17272 = ADVANCED_FACE ( 'NONE', ( #15910 ), #7130, .F. ) ;
#17273 = EDGE_CURVE ( 'NONE', #11167, #20475, #809, .T. ) ;
#17274 = CARTESIAN_POINT ( 'NONE',  ( -178.0837196006577585, 111.1705890210531322, 28.96620944385036722 ) ) ;
#17275 = CARTESIAN_POINT ( 'NONE',  ( -38.52381090778946060, 128.7773429936079310, -17.17645200753749180 ) ) ;
#17276 = DIRECTION ( 'NONE',  ( 1.000000000000000000, 0.000000000000000000, 0.000000000000000000 ) ) ;
#17277 = ORIENTED_EDGE ( 'NONE', *, *, #1563, .F. ) ;
#17278 = CARTESIAN_POINT ( 'NONE',  ( 1.982541115402066017E-14, -150.0000000000000568, -100.0000000000000142 ) ) ;
#17279 = ORIENTED_EDGE ( 'NONE', *, *, #20956, .F. ) ;
#17280 = DIRECTION ( 'NONE',  ( -0.000000000000000000, -0.000000000000000000, -1.000000000000000000 ) ) ;
#17281 = CARTESIAN_POINT ( 'NONE',  ( -191.3917181558073253, 102.3917013931790478, -32.04925462112321100 ) ) ;
#17282 = EDGE_LOOP ( 'NONE', ( #4760, #104, #9983, #483, #23649, #21063, #20165, #261 ) ) ;
#17283 = VECTOR ( 'NONE', #662, 1000.000000000000000 ) ;
#17284 = EDGE_LOOP ( 'NONE', ( #25774, #27068, #23756, #21304 ) ) ;
#17285 = CARTESIAN_POINT ( 'NONE',  ( 157.4999999999998579, 115.9231871884577174, -45.00000000000000000 ) ) ;
#17286 = ORIENTED_EDGE ( 'NONE', *, *, #17136, .T. ) ;
#17287 = ORIENTED_EDGE ( 'NONE', *, *, #21976, .T. ) ;
#17288 = ORIENTED_EDGE ( 'NONE', *, *, #6323, .T. ) ;
#17289 = EDGE_CURVE ( 'NONE', #17818, #27311, #7275, .T. ) ;
#17290 = EDGE_CURVE ( 'NONE', #1600, #13603, #11456, .T. ) ;
#17291 = PLANE ( 'NONE',  #14490 ) ;
#17292 = EDGE_CURVE ( 'NONE', #24530, #20507, #11881, .T. ) ;
#17293 = DIRECTION ( 'NONE',  ( 0.000000000000000000, -1.000000000000000000, 0.000000000000000000 ) ) ;
#17294 = CARTESIAN_POINT ( 'NONE',  ( 157.4999999999998579, 161.0649373235845019, 45.00000000000000000 ) ) ;
#17295 = DIRECTION ( 'NONE',  ( 0.000000000000000000, -1.000000000000000000, 0.000000000000000000 ) ) ;
#17296 = DIRECTION ( 'NONE',  ( -0.8916010070298868717, -0.4528218681372309651, 0.000000000000000000 ) ) ;
#17297 = CARTESIAN_POINT ( 'NONE',  ( -223.9727688501994578, 61.67225750692603015, -20.13450274023890785 ) ) ;
#17298 = ORIENTED_EDGE ( 'NONE', *, *, #9379, .T. ) ;
#17299 = DIRECTION ( 'NONE',  ( -0.000000000000000000, -1.000000000000000000, -0.000000000000000000 ) ) ;
#17300 = FACE_OUTER_BOUND ( 'NONE', #8631, .T. ) ;
#17301 = CARTESIAN_POINT ( 'NONE',  ( 157.9999999999997726, 248.5866250825770294, 45.00000000000000000 ) ) ;
#17302 = FACE_OUTER_BOUND ( 'NONE', #6676, .T. ) ;
#17303 = VECTOR ( 'NONE', #15715, 1000.000000000000000 ) ;
#17304 = VERTEX_POINT ( 'NONE', #22788 ) ;
#17305 = CARTESIAN_POINT ( 'NONE',  ( -215.7935364303658901, 60.28281843632711912, 13.31033261678752844 ) ) ;
#17306 = VECTOR ( 'NONE', #27113, 1000.000000000000000 ) ;
#17307 = PLANE ( 'NONE',  #17108 ) ;
#17308 = CARTESIAN_POINT ( 'NONE',  ( 9.999999999999964473, 60.00000000000001421, 80.00000000000001421 ) ) ;
#17309 = DIRECTION ( 'NONE',  ( 0.8916010070297751833, 0.4528218681374507892, 0.000000000000000000 ) ) ;
#17310 = LINE ( 'NONE', #26351, #25292 ) ;
#17311 = DIRECTION ( 'NONE',  ( -0.8916010070298766577, -0.4528218681372509491, 0.000000000000000000 ) ) ;
#17312 = VERTEX_POINT ( 'NONE', #20625 ) ;
#17313 = CARTESIAN_POINT ( 'NONE',  ( 158.0000000000001421, 193.4133749174225443, 45.00000000000000000 ) ) ;
#17314 = VERTEX_POINT ( 'NONE', #9713 ) ;
#17315 = CARTESIAN_POINT ( 'NONE',  ( -254.3350114625770289, -91.18033988749901653, -16.36034929305424512 ) ) ;
#17316 = ORIENTED_EDGE ( 'NONE', *, *, #19565, .F. ) ;
#17317 = ORIENTED_EDGE ( 'NONE', *, *, #9657, .F. ) ;
#17318 = FACE_OUTER_BOUND ( 'NONE', #1497, .T. ) ;
#17319 = AXIS2_PLACEMENT_3D ( 'NONE', #16845, #27600, #4039 ) ;
#17320 = ORIENTED_EDGE ( 'NONE', *, *, #25863, .F. ) ;
#17321 = EDGE_CURVE ( 'NONE', #9638, #26421, #14877, .T. ) ;
#17322 = ORIENTED_EDGE ( 'NONE', *, *, #26341, .F. ) ;
#17323 = DIRECTION ( 'NONE',  ( 1.000000000000000000, 0.000000000000000000, 0.000000000000000000 ) ) ;
#17324 = VECTOR ( 'NONE', #19235, 1000.000000000000114 ) ;
#17325 = CARTESIAN_POINT ( 'NONE',  ( -143.9457187202836792, 125.8028027456154234, -18.55619470350388411 ) ) ;
#17326 = FACE_OUTER_BOUND ( 'NONE', #10972, .T. ) ;
#17327 = ADVANCED_FACE ( 'NONE', ( #1226 ), #20643, .T. ) ;
#17328 = EDGE_CURVE ( 'NONE', #5281, #800, #1505, .T. ) ;
#17329 = CARTESIAN_POINT ( 'NONE',  ( -156.8436863811591593, 180.7779002010535407, -15.00000000000000000 ) ) ;
#17330 = PLANE ( 'NONE',  #21989 ) ;
#17331 = DIRECTION ( 'NONE',  ( 0.4528218681382907285, -0.8916010070293486356, 0.000000000000000000 ) ) ;
#17332 = CARTESIAN_POINT ( 'NONE',  ( -268.0371306804030951, -170.6155949349647756, 94.25159887050631369 ) ) ;
#17333 = CARTESIAN_POINT ( 'NONE',  ( -231.9378824387723057, 93.53122965655593646, -12.99999999999999645 ) ) ;
#17334 = FACE_OUTER_BOUND ( 'NONE', #25273, .T. ) ;
#17335 = CARTESIAN_POINT ( 'NONE',  ( 5.999999999999998224, 6.123233995736766282E-16, -5.000000000000000000 ) ) ;
#17336 = CARTESIAN_POINT ( 'NONE',  ( 157.4999999999998010, 241.3169375638095460, 45.00000000000000000 ) ) ;
#17337 = LINE ( 'NONE', #11026, #17814 ) ;
#17338 = DIRECTION ( 'NONE',  ( 0.000000000000000000, 0.000000000000000000, 1.000000000000000000 ) ) ;
#17339 = EDGE_LOOP ( 'NONE', ( #11008, #16827, #10318, #18412 ) ) ;
#17340 = LINE ( 'NONE', #13472, #10583 ) ;
#17341 = CIRCLE ( 'NONE', #4953, 29.99999999999999645 ) ;
#17342 = AXIS2_PLACEMENT_3D ( 'NONE', #10665, #8933, #19425 ) ;
#17343 = CYLINDRICAL_SURFACE ( 'NONE', #12398, 10.00000000000000888 ) ;
#17344 = LINE ( 'NONE', #10605, #8011 ) ;
#17345 = CARTESIAN_POINT ( 'NONE',  ( -270.1025481742786951, -91.18033988749901653, 14.95564396479129243 ) ) ;
#17346 = ORIENTED_EDGE ( 'NONE', *, *, #14413, .F. ) ;
#17347 = CARTESIAN_POINT ( 'NONE',  ( 92.84236432024516716, 239.7913859916932040, -17.77233924293991407 ) ) ;
#17348 = ORIENTED_EDGE ( 'NONE', *, *, #9378, .T. ) ;
#17349 = CARTESIAN_POINT ( 'NONE',  ( 6.333949844049013400, 140.1907388332623725, -13.00000000000000355 ) ) ;
#17350 = VERTEX_POINT ( 'NONE', #20905 ) ;
#17351 = ORIENTED_EDGE ( 'NONE', *, *, #15203, .T. ) ;
#17352 = EDGE_CURVE ( 'NONE', #8916, #17036, #25497, .T. ) ;
#17353=STYLED_ITEM('',(#28427),#28013);
#17354 = EDGE_LOOP ( 'NONE', ( #17418, #6328, #7003, #3763, #3148, #8169 ) ) ;
#17355 = EDGE_LOOP ( 'NONE', ( #16253, #8662, #13962, #2718 ) ) ;
#17356 = ORIENTED_EDGE ( 'NONE', *, *, #24112, .T. ) ;
#17357 = DIRECTION ( 'NONE',  ( 1.000000000000000000, 0.000000000000000000, -0.000000000000000000 ) ) ;
#17358 = EDGE_CURVE ( 'NONE', #21631, #10760, #9992, .T. ) ;
#17359 = AXIS2_PLACEMENT_3D ( 'NONE', #28378, #3978, #15201 ) ;
#17360 = ADVANCED_FACE ( 'NONE', ( #19031 ), #22941, .T. ) ;
#17361 = VECTOR ( 'NONE', #16087, 1000.000000000000000 ) ;
#17362 = LINE ( 'NONE', #4292, #4564 ) ;
#17363 = CARTESIAN_POINT ( 'NONE',  ( 157.4999999999998579, 58.24206201579573872, -45.00000000000000000 ) ) ;
#17364 = CARTESIAN_POINT ( 'NONE',  ( -42.99650729631200363, 71.03850157808263077, 99.00000000000000000 ) ) ;
#17365 = PLANE ( 'NONE',  #7619 ) ;
#17366 = CARTESIAN_POINT ( 'NONE',  ( 49.56615429303207065, 203.2034914284457159, 12.99999999999999822 ) ) ;
#17367 = DIRECTION ( 'NONE',  ( -0.000000000000000000, -0.000000000000000000, -1.000000000000000000 ) ) ;
#17368 = CARTESIAN_POINT ( 'NONE',  ( 157.9999999999996589, 281.1890001801680796, 45.00000000000000000 ) ) ;
#17369 = DIRECTION ( 'NONE',  ( -0.000000000000000000, -0.000000000000000000, -1.000000000000000000 ) ) ;
#17371 = PLANE ( 'NONE',  #7749 ) ;
#17370 = VECTOR ( 'NONE', #10426, 1000.000000000000000 ) ;
#17372 = LINE ( 'NONE', #18382, #21995 ) ;
#17373 = DIRECTION ( 'NONE',  ( 0.000000000000000000, 0.000000000000000000, -1.000000000000000000 ) ) ;
#17374 = DIRECTION ( 'NONE',  ( 0.000000000000000000, -1.000000000000000000, 0.000000000000000000 ) ) ;
#17376 = EDGE_LOOP ( 'NONE', ( #25941, #2397, #26877, #17490, #14964 ) ) ;
#17375 = VERTEX_POINT ( 'NONE', #23626 ) ;
#17377 = CARTESIAN_POINT ( 'NONE',  ( -232.1441312129731500, 91.01446451744486410, -15.02668720701366212 ) ) ;
#17378 = VECTOR ( 'NONE', #6175, 1000.000000000000000 ) ;
#17379 = PRODUCT_DEFINITION_SHAPE ( 'NONE', 'NONE',  #16857 ) ;
#17380 = AXIS2_PLACEMENT_3D ( 'NONE', #10343, #10484, #19103 ) ;
#17381 = CARTESIAN_POINT ( 'NONE',  ( -263.2300671076336016, -166.3683464297101580, -109.9999999999998721 ) ) ;
#17382 = ORIENTED_EDGE ( 'NONE', *, *, #15147, .F. ) ;
#17383 = PRODUCT_CONTEXT ( 'NONE', #3578, 'mechanical' ) ;
#17384 = EDGE_CURVE ( 'NONE', #24450, #7154, #19729, .T. ) ;
#17385 = VERTEX_POINT ( 'NONE', #8117 ) ;
#17387 = ORIENTED_EDGE ( 'NONE', *, *, #22638, .F. ) ;
#17386 = AXIS2_PLACEMENT_3D ( 'NONE', #5633, #23300, #27314 ) ;
#17388 = EDGE_CURVE ( 'NONE', #6791, #8829, #12724, .T. ) ;
#17389 = CARTESIAN_POINT ( 'NONE',  ( -222.0211651016019516, 135.7213904098416890, -12.97555235349485869 ) ) ;
#17390 = DIRECTION ( 'NONE',  ( -1.000000000000000000, 0.000000000000000000, 0.000000000000000000 ) ) ;
#17391 = ORIENTED_EDGE ( 'NONE', *, *, #24179, .T. ) ;
#17392 = CARTESIAN_POINT ( 'NONE',  ( 89.77759941121082932, 81.13568025369244197, -100.0000000000000142 ) ) ;
#17393 = VECTOR ( 'NONE', #2459, 1000.000000000000000 ) ;
#17394 = EDGE_CURVE ( 'NONE', #19844, #1242, #13794, .T. ) ;
#17395 = CARTESIAN_POINT ( 'NONE',  ( 158.0000000000010232, 108.1456246621830957, 45.00000000000000000 ) ) ;
#17396 = VECTOR ( 'NONE', #11557, 1000.000000000000000 ) ;
#17397 = VERTEX_POINT ( 'NONE', #12162 ) ;
#17398 = CARTESIAN_POINT ( 'NONE',  ( -227.2146340703364160, 90.21260626941095495, 15.67423580940634231 ) ) ;
#17399 = ORIENTED_EDGE ( 'NONE', *, *, #22847, .F. ) ;
#17400 = FACE_OUTER_BOUND ( 'NONE', #8306, .T. ) ;
#17401 = AXIS2_PLACEMENT_3D ( 'NONE', #19646, #12770, #28251 ) ;
#17402 = EDGE_CURVE ( 'NONE', #20915, #16382, #27779, .T. ) ;
#17403 = CARTESIAN_POINT ( 'NONE',  ( -37.82257053376181233, 71.03850157808263077, 99.00000000000000000 ) ) ;
#17404 = DIRECTION ( 'NONE',  ( 0.000000000000000000, 0.000000000000000000, 1.000000000000000000 ) ) ;
#17405 = AXIS2_PLACEMENT_3D ( 'NONE', #22421, #6758, #18118 ) ;
#17406 = CARTESIAN_POINT ( 'NONE',  ( 158.0000000000009948, 110.6534996696901345, 45.00000000000000000 ) ) ;
#17407 = EDGE_LOOP ( 'NONE', ( #6814, #13412, #14304, #15855 ) ) ;
#17408 = CARTESIAN_POINT ( 'NONE',  ( 117.2377723979408017, 206.1768395233783338, 99.61817846761982764 ) ) ;
#17409 = CARTESIAN_POINT ( 'NONE',  ( 158.0000000000010516, 103.6377496546760568, -45.00000000000000000 ) ) ;
#17410 = DIRECTION ( 'NONE',  ( 5.551115123125777969E-15, 0.000000000000000000, 1.000000000000000000 ) ) ;
#17411 = CARTESIAN_POINT ( 'NONE',  ( 33.10302365956999182, 221.6666220619077876, -15.00000000000000000 ) ) ;
#17412 = VERTEX_POINT ( 'NONE', #14588 ) ;
#17413 = EDGE_CURVE ( 'NONE', #18824, #7691, #3671, .T. ) ;
#17414 = DIRECTION ( 'NONE',  ( 0.4528218681369524101, 0.8916010070300282031, -0.000000000000000000 ) ) ;
#17415 = AXIS2_PLACEMENT_3D ( 'NONE', #25565, #20980, #19111 ) ;
#17416 = LINE ( 'NONE', #13401, #19871 ) ;
#17417 = CARTESIAN_POINT ( 'NONE',  ( -203.7125816754261791, 92.59027862332997927, 28.49518943040505192 ) ) ;
#17418 = ORIENTED_EDGE ( 'NONE', *, *, #20728, .T. ) ;
#17419 = ORIENTED_EDGE ( 'NONE', *, *, #3994, .F. ) ;
#17420 = AXIS2_PLACEMENT_3D ( 'NONE', #8129, #21196, #3241 ) ;
#17421 = ADVANCED_FACE ( 'NONE', ( #17014 ), #27638, .F. ) ;
#17422 = LINE ( 'NONE', #11103, #7447 ) ;
#17423 = CARTESIAN_POINT ( 'NONE',  ( -164.5307643740429455, 118.5035042282064097, -22.94257969500540995 ) ) ;
#17424 = VERTEX_POINT ( 'NONE', #5535 ) ;
#17425 = VERTEX_POINT ( 'NONE', #12443 ) ;
#17426 = CARTESIAN_POINT ( 'NONE',  ( 12.78000883847031588, 237.8887863075477469, -45.00000000000000000 ) ) ;
#17427 = CARTESIAN_POINT ( 'NONE',  ( 158.0000000000011937, 93.09837461714084839, -45.00000000000000000 ) ) ;
#17428 = ORIENTED_EDGE ( 'NONE', *, *, #17914, .T. ) ;
#17429 = VERTEX_POINT ( 'NONE', #5955 ) ;
#17430 = CARTESIAN_POINT ( 'NONE',  ( 1.569447331094923070, 135.1286268723246167, 15.37625018068031757 ) ) ;
#17431 = EDGE_CURVE ( 'NONE', #19692, #27184, #21040, .T. ) ;
#17432 = ADVANCED_FACE ( 'NONE', ( #23483 ), #3937, .T. ) ;
#17433 = AXIS2_PLACEMENT_3D ( 'NONE', #671, #6977, #945 ) ;
#17434 = FACE_OUTER_BOUND ( 'NONE', #7215, .T. ) ;
#17435 = DIRECTION ( 'NONE',  ( -0.000000000000000000, -0.000000000000000000, -1.000000000000000000 ) ) ;
#17436 = DIRECTION ( 'NONE',  ( -0.000000000000000000, -0.000000000000000000, -1.000000000000000000 ) ) ;
#17437 = DIRECTION ( 'NONE',  ( 0.000000000000000000, 0.000000000000000000, -1.000000000000000000 ) ) ;
#17438 = CIRCLE ( 'NONE', #2755, 6.000000000000005329 ) ;
#17439 = DIRECTION ( 'NONE',  ( -1.000000000000000000, -2.602085213965211135E-16, 0.000000000000000000 ) ) ;
#17440 = EDGE_LOOP ( 'NONE', ( #13159, #20856, #14142, #3102 ) ) ;
#17441 = DIRECTION ( 'NONE',  ( 1.000000000000000000, 0.000000000000000000, -0.000000000000000000 ) ) ;
#17442 = CARTESIAN_POINT ( 'NONE',  ( 156.9574749595459764, 213.0812361363529988, -45.00000000000000000 ) ) ;
#17443 = CARTESIAN_POINT ( 'NONE',  ( 158.0000000000005400, 155.7952498048169048, 45.00000000000000000 ) ) ;
#17444 = DIRECTION ( 'NONE',  ( -0.8916010070297142320, -0.4528218681375706933, 0.000000000000000000 ) ) ;
#17445 = ORIENTED_EDGE ( 'NONE', *, *, #6390, .F. ) ;
#17446 = EDGE_CURVE ( 'NONE', #366, #17857, #3796, .T. ) ;
#17447 = DIRECTION ( 'NONE',  ( 1.000000000000000000, -0.000000000000000000, -0.000000000000000000 ) ) ;
#17448 = CARTESIAN_POINT ( 'NONE',  ( 158.0000000000009663, 113.6692496847042264, -45.00000000000000000 ) ) ;
#17449 = CARTESIAN_POINT ( 'NONE',  ( -273.6135038633245244, -165.0000000000001705, 86.76553013670502423 ) ) ;
#17450 = CARTESIAN_POINT ( 'NONE',  ( -277.2150368962633706, -237.2150368962634559, 105.0000000000000000 ) ) ;
#17451 = DIRECTION ( 'NONE',  ( -3.469446951953614189E-16, 1.000000000000000000, -0.000000000000000000 ) ) ;
#17452 = LINE ( 'NONE', #6681, #22580 ) ;
#17453 = ORIENTED_EDGE ( 'NONE', *, *, #24991, .T. ) ;
#17454 = ADVANCED_FACE ( 'NONE', ( #19168 ), #1776, .F. ) ;
#17455 = VECTOR ( 'NONE', #12164, 1000.000000000000227 ) ;
#17456 = FACE_OUTER_BOUND ( 'NONE', #14758, .T. ) ;
#17457 = ORIENTED_EDGE ( 'NONE', *, *, #14581, .T. ) ;
#17458 = PLANE ( 'NONE',  #23201 ) ;
#17459 = ORIENTED_EDGE ( 'NONE', *, *, #9909, .T. ) ;
#17460 = EDGE_CURVE ( 'NONE', #14958, #2723, #6275, .T. ) ;
#17461 = VERTEX_POINT ( 'NONE', #15049 ) ;
#17462 = DIRECTION ( 'NONE',  ( -0.000000000000000000, -0.000000000000000000, -1.000000000000000000 ) ) ;
#17463 = AXIS2_PLACEMENT_3D ( 'NONE', #24667, #11614, #23315 ) ;
#17464 = ORIENTED_EDGE ( 'NONE', *, *, #6943, .T. ) ;
#17465 = VERTEX_POINT ( 'NONE', #3833 ) ;
#17466 = CARTESIAN_POINT ( 'NONE',  ( 157.9999999999999147, 215.9842499849850697, 45.00000000000000000 ) ) ;
#17467 = CARTESIAN_POINT ( 'NONE',  ( 52.57751368840760620, 248.9624084326366358, -45.00000000000000000 ) ) ;
#17468 = CARTESIAN_POINT ( 'NONE',  ( -213.1827219047386848, -216.7767438708612531, 95.00000000000004263 ) ) ;
#17469 = DIRECTION ( 'NONE',  ( -0.000000000000000000, -0.000000000000000000, 1.000000000000000000 ) ) ;
#17470 = CARTESIAN_POINT ( 'NONE',  ( 157.4999999999998579, 90.84443711338730054, 45.00000000000000000 ) ) ;
#17471 = CARTESIAN_POINT ( 'NONE',  ( -260.0000000000001137, -157.0000000000000284, 110.0000000000000142 ) ) ;
#17472 = DIRECTION ( 'NONE',  ( -0.8916010070296429557, 0.4528218681377111920, 0.000000000000000000 ) ) ;
#17473 = CARTESIAN_POINT ( 'NONE',  ( -221.9298065274946339, 88.28604124582930979, -17.46722815149482599 ) ) ;
#17474 = VECTOR ( 'NONE', #8224, 999.9999999999998863 ) ;
#17475 = CARTESIAN_POINT ( 'NONE',  ( 158.0000000000008811, 123.1928747072253572, 45.00000000000000000 ) ) ;
#17476 = LINE ( 'NONE', #8722, #9433 ) ;
#17477 = LINE ( 'NONE', #13615, #14763 ) ;
#17478 = CARTESIAN_POINT ( 'NONE',  ( 179.9999999999999147, -150.0000000000000284, -100.0000000000000142 ) ) ;
#17479 = CARTESIAN_POINT ( 'NONE',  ( 157.4999999999998579, 220.0000000000000284, -99.00000000000001421 ) ) ;
#17480 = ORIENTED_EDGE ( 'NONE', *, *, #4780, .T. ) ;
#17481 = CARTESIAN_POINT ( 'NONE',  ( 158.0000000000013927, 75.54324956459154805, -45.00000000000000000 ) ) ;
#17482 = CIRCLE ( 'NONE', #7412, 7.999999999999979572 ) ;
#17483 = CARTESIAN_POINT ( 'NONE',  ( 110.2602732333167808, 140.0000000000000000, 92.61747884359283489 ) ) ;
#17484 = CARTESIAN_POINT ( 'NONE',  ( 158.0000000000010232, 108.1456246621830957, 45.00000000000000000 ) ) ;
#17485 = CARTESIAN_POINT ( 'NONE',  ( 107.2641058044744682, 208.5632379335606004, -140.4781857268138765 ) ) ;
#17486 = VERTEX_POINT ( 'NONE', #1542 ) ;
#17487 = EDGE_CURVE ( 'NONE', #14163, #27184, #14486, .T. ) ;
#17488 = CARTESIAN_POINT ( 'NONE',  ( 102.0190107526883310, 244.0003474240100161, -16.44012727446676791 ) ) ;
#17489 = VERTEX_POINT ( 'NONE', #12622 ) ;
#17490 = ORIENTED_EDGE ( 'NONE', *, *, #4944, .T. ) ;
#17491 = ORIENTED_EDGE ( 'NONE', *, *, #10219, .F. ) ;
#17492 = VECTOR ( 'NONE', #28377, 1000.000000000000000 ) ;
#17493 = ORIENTED_EDGE ( 'NONE', *, *, #12971, .F. ) ;
#17494 = ORIENTED_EDGE ( 'NONE', *, *, #2804, .T. ) ;
#17495 = DIRECTION ( 'NONE',  ( -0.000000000000000000, -1.000000000000000000, -0.000000000000000000 ) ) ;
#17496 = AXIS2_PLACEMENT_3D ( 'NONE', #26635, #24921, #18319 ) ;
#17497 = CARTESIAN_POINT ( 'NONE',  ( 158.0000000000000000, 208.4606249624626457, 45.00000000000000000 ) ) ;
#17498 = VECTOR ( 'NONE', #15924, 999.9999999999998863 ) ;
#17499 = EDGE_CURVE ( 'NONE', #16958, #21312, #8150, .T. ) ;
#17500 = DIRECTION ( 'NONE',  ( 1.000000000000000000, 0.000000000000000000, -0.000000000000000000 ) ) ;
#17501 = DIRECTION ( 'NONE',  ( -0.000000000000000000, -1.000000000000000000, -0.000000000000000000 ) ) ;
#17502 = CARTESIAN_POINT ( 'NONE',  ( -216.4559255058941289, 59.30400871604422264, 28.11406665935853866 ) ) ;
#17503 = CARTESIAN_POINT ( 'NONE',  ( 187.4999999999996305, 40.68693696324645970, 45.00000000000000000 ) ) ;
#17504 = LINE ( 'NONE', #6596, #6228 ) ;
#17505 = EDGE_CURVE ( 'NONE', #13208, #19162, #1398, .T. ) ;
#17506 = DIRECTION ( 'NONE',  ( -1.000000000000000000, 0.000000000000000000, -9.251858538542974046E-17 ) ) ;
#17507 = DIRECTION ( 'NONE',  ( 0.000000000000000000, -1.000000000000000000, 0.000000000000000000 ) ) ;
#17508 = LINE ( 'NONE', #26276, #10460 ) ;
#17509 = DIRECTION ( 'NONE',  ( -0.000000000000000000, 0.000000000000000000, -1.000000000000000000 ) ) ;
#17510 = AXIS2_PLACEMENT_3D ( 'NONE', #14423, #14989, #23736 ) ;
#17511 = CARTESIAN_POINT ( 'NONE',  ( -38.50235330400180089, 128.7731110165481141, 17.17814592602437429 ) ) ;
#17512 = DIRECTION ( 'NONE',  ( -0.000000000000000000, -0.000000000000000000, 1.000000000000000000 ) ) ;
#17513 = DIRECTION ( 'NONE',  ( 0.4528218681373720744, 0.8916010070298151513, -0.000000000000000000 ) ) ;
#17514 = ADVANCED_FACE ( 'NONE', ( #10171 ), #11494, .T. ) ;
#17515 = LINE ( 'NONE', #24139, #26271 ) ;
#17516 = VECTOR ( 'NONE', #7406, 1000.000000000000000 ) ;
#17518 = EDGE_LOOP ( 'NONE', ( #22411, #18804, #28255, #27043 ) ) ;
#17517 = ORIENTED_EDGE ( 'NONE', *, *, #2266, .T. ) ;
#17519 = AXIS2_PLACEMENT_3D ( 'NONE', #20848, #1445, #18418 ) ;
#17520 = CARTESIAN_POINT ( 'NONE',  ( -178.5327134719260869, 110.5652120027505703, 30.30295336851717991 ) ) ;
#17521 = EDGE_CURVE ( 'NONE', #17838, #11217, #1680, .T. ) ;
#17522 = CIRCLE ( 'NONE', #12052, 2.000000000000000444 ) ;
#17523 = ADVANCED_FACE ( 'NONE', ( #25809 ), #12134, .T. ) ;
#17524 = DIRECTION ( 'NONE',  ( 0.000000000000000000, -0.000000000000000000, -1.000000000000000000 ) ) ;
#17525 = ORIENTED_EDGE ( 'NONE', *, *, #10004, .F. ) ;
#17526 = ORIENTED_EDGE ( 'NONE', *, *, #10935, .F. ) ;
#17527 = EDGE_LOOP ( 'NONE', ( #27578, #14976, #19784, #3993 ) ) ;
#17528 = DIRECTION ( 'NONE',  ( 0.000000000000000000, 0.000000000000000000, 1.000000000000000000 ) ) ;
#17529 = LINE ( 'NONE', #15396, #27349 ) ;
#17530 = ORIENTED_EDGE ( 'NONE', *, *, #12258, .F. ) ;
#17531 = B_SPLINE_CURVE_WITH_KNOTS ( 'NONE', 3,
 ( #15897, #22639, #6965, #9563, #11440, #932, #515, #2798 ),
 .UNSPECIFIED., .F., .F.,
 ( 4, 2, 2, 4 ),
 ( 0.000000000000000000, 0.004190943542067912184, 0.008381887084135824367, 0.01676377416827165567 ),
 .UNSPECIFIED. ) ;
#17532 = AXIS2_PLACEMENT_3D ( 'NONE', #626, #25166, #20296 ) ;
#17533 = CARTESIAN_POINT ( 'NONE',  ( 157.4999999999998579, 55.73418700828869277, -45.00000000000000000 ) ) ;
#17534 = CIRCLE ( 'NONE', #8823, 66.76834224489934400 ) ;
#17535 = CARTESIAN_POINT ( 'NONE',  ( -203.1779787704217313, 93.05164332230201296, -28.77272332722132475 ) ) ;
#17536 = ORIENTED_EDGE ( 'NONE', *, *, #4631, .F. ) ;
#17537 = CARTESIAN_POINT ( 'NONE',  ( -228.4379895967119012, 88.56164859814569468, 15.57174740462524909 ) ) ;
#17538 = AXIS2_PLACEMENT_3D ( 'NONE', #17758, #11312, #26813 ) ;
#17539 = CARTESIAN_POINT ( 'NONE',  ( -210.8169819562698137, -219.6631312228495858, 108.5590195769788551 ) ) ;
#17540 = VECTOR ( 'NONE', #3280, 1000.000000000000000 ) ;
#17541 = CARTESIAN_POINT ( 'NONE',  ( 157.9999999999996874, 264.1417501351260171, 45.00000000000000000 ) ) ;
#17542 = CARTESIAN_POINT ( 'NONE',  ( 158.7697712239360044, 201.6949277321624550, -149.5176478624189826 ) ) ;
#17543 = EDGE_CURVE ( 'NONE', #19790, #4525, #26652, .T. ) ;
#17544 = EDGE_CURVE ( 'NONE', #16772, #25545, #15611, .T. ) ;
#17545 = VERTEX_POINT ( 'NONE', #6562 ) ;
#17546 = CARTESIAN_POINT ( 'NONE',  ( 119.1208832861755269, 204.0157960616585910, 100.0000000000002274 ) ) ;
#17547 = CARTESIAN_POINT ( 'NONE',  ( 157.9999999999996874, 266.1417501351260171, 45.00000000000000000 ) ) ;
#17548 = FACE_OUTER_BOUND ( 'NONE', #5283, .T. ) ;
#17549 = LINE ( 'NONE', #611, #23591 ) ;
#17550 = ORIENTED_EDGE ( 'NONE', *, *, #6181, .T. ) ;
#17551 = AXIS2_PLACEMENT_3D ( 'NONE', #16909, #19342, #25663 ) ;
#17552 = CARTESIAN_POINT ( 'NONE',  ( -211.4344004814429923, -220.0000000000001137, -107.6907272673696383 ) ) ;
#17553 = AXIS2_PLACEMENT_3D ( 'NONE', #9624, #17951, #15666 ) ;
#17554 = EDGE_CURVE ( 'NONE', #5169, #14223, #2519, .T. ) ;
#17555 = DIRECTION ( 'NONE',  ( 1.850371707708594316E-16, -1.000000000000000000, 0.000000000000000000 ) ) ;
#17556 = LINE ( 'NONE', #24599, #28206 ) ;
#17557 = VERTEX_POINT ( 'NONE', #6698 ) ;
#17558 =( LENGTH_UNIT ( ) NAMED_UNIT ( * ) SI_UNIT ( .MILLI., .METRE. ) );
#17559 = CONICAL_SURFACE ( 'NONE', #5181, 5.999999999999977796, 1.029744258676652979 ) ;
#17560 = ORIENTED_EDGE ( 'NONE', *, *, #27083, .F. ) ;
#17561 = VECTOR ( 'NONE', #7296, 1000.000000000000000 ) ;
#17562 = EDGE_CURVE ( 'NONE', #25296, #7114, #4532, .T. ) ;
#17563 = LINE ( 'NONE', #23896, #23020 ) ;
#17564 = CARTESIAN_POINT ( 'NONE',  ( -175.0822582904459921, 112.9350779648750489, -28.38028793360534507 ) ) ;
#17565 = ORIENTED_EDGE ( 'NONE', *, *, #6337, .F. ) ;
#17566 = VERTEX_POINT ( 'NONE', #6419 ) ;
#17567 = CARTESIAN_POINT ( 'NONE',  ( -115.3221550338875971, 71.54464929955099706, 82.80879831960034210 ) ) ;
#17568 = CARTESIAN_POINT ( 'NONE',  ( 157.9999999999999716, 208.9684999699701393, -45.00000000000000000 ) ) ;
#17569 = ORIENTED_EDGE ( 'NONE', *, *, #10889, .T. ) ;
#17570 = ORIENTED_EDGE ( 'NONE', *, *, #24100, .T. ) ;
#17571 = VECTOR ( 'NONE', #1043, 999.9999999999998863 ) ;
#17572 = DIRECTION ( 'NONE',  ( 1.000000000000000000, -0.000000000000000000, -0.000000000000000000 ) ) ;
#17573 = AXIS2_PLACEMENT_3D ( 'NONE', #4472, #19712, #17699 ) ;
#17574 = CARTESIAN_POINT ( 'NONE',  ( 157.9999999999997442, 253.6023750975910502, 45.00000000000000000 ) ) ;
#17575 = DIRECTION ( 'NONE',  ( -0.8916010070295511403, 0.4528218681378916033, 0.000000000000000000 ) ) ;
#17576 = FACE_OUTER_BOUND ( 'NONE', #22020, .T. ) ;
#17577 = AXIS2_PLACEMENT_3D ( 'NONE', #22968, #7740, #14080 ) ;
#17578 = LINE ( 'NONE', #11417, #27006 ) ;
#17579 = DIRECTION ( 'NONE',  ( -1.000000000000000000, 0.000000000000000000, 0.000000000000000000 ) ) ;
#17580 = CARTESIAN_POINT ( 'NONE',  ( 157.4999999999998579, 113.4153121809506786, 45.00000000000000000 ) ) ;
#17581 = ADVANCED_FACE ( 'NONE', ( #15768 ), #13610, .F. ) ;
#17582 = ORIENTED_EDGE ( 'NONE', *, *, #1414, .F. ) ;
#17583 = CARTESIAN_POINT ( 'NONE',  ( 119.9999999999999005, 203.2294901687515960, -100.0000000000000142 ) ) ;
#17584 = CARTESIAN_POINT ( 'NONE',  ( 157.4999999999997442, 256.3641876088515232, 45.00000000000000000 ) ) ;
#17585 = PLANE ( 'NONE',  #21053 ) ;
#17586 = DIRECTION ( 'NONE',  ( -1.321694076934710155E-16, 1.000000000000000000, 0.000000000000000000 ) ) ;
#17587 = VERTEX_POINT ( 'NONE', #19634 ) ;
#17588 = LINE ( 'NONE', #358, #10510 ) ;
#17589 = ORIENTED_EDGE ( 'NONE', *, *, #15870, .T. ) ;
#17590 = DIRECTION ( 'NONE',  ( 0.000000000000000000, 0.000000000000000000, 1.000000000000000000 ) ) ;
#17591 = LINE ( 'NONE', #28348, #11932 ) ;
#17592 = FACE_OUTER_BOUND ( 'NONE', #6720, .T. ) ;
#17593 = LINE ( 'NONE', #1794, #9245 ) ;
#17594 = CARTESIAN_POINT ( 'NONE',  ( 157.9999999999997158, 261.6338751276190351, 45.00000000000000000 ) ) ;
#17595 = ORIENTED_EDGE ( 'NONE', *, *, #9091, .F. ) ;
#17596 = AXIS2_PLACEMENT_3D ( 'NONE', #25585, #23441, #21285 ) ;
#17597 = EDGE_CURVE ( 'NONE', #4287, #24562, #21794, .T. ) ;
#17598 = VECTOR ( 'NONE', #4338, 1000.000000000000000 ) ;
#17599 = CARTESIAN_POINT ( 'NONE',  ( -209.7480663293921452, 74.08843928001617485, 34.98546963098892348 ) ) ;
#17600 = ORIENTED_EDGE ( 'NONE', *, *, #8134, .F. ) ;
#17601 = EDGE_CURVE ( 'NONE', #27317, #8030, #6878, .T. ) ;
#17602 = CARTESIAN_POINT ( 'NONE',  ( 157.9999999999997726, 241.5708750675630370, 45.00000000000000000 ) ) ;
#17603 = VERTEX_POINT ( 'NONE', #8718 ) ;
#17604 = AXIS2_PLACEMENT_3D ( 'NONE', #25055, #18722, #22896 ) ;
#17605 = EDGE_LOOP ( 'NONE', ( #28018, #3276, #19862, #28191 ) ) ;
#17606 = LINE ( 'NONE', #6407, #28247 ) ;
#17607 = VERTEX_POINT ( 'NONE', #4398 ) ;
#17608 = ORIENTED_EDGE ( 'NONE', *, *, #3921, .F. ) ;
#17609 = CARTESIAN_POINT ( 'NONE',  ( -224.0127348693837916, 134.1242697789051306, 15.11921763784017969 ) ) ;
#17610 = EDGE_CURVE ( 'NONE', #13525, #22223, #6983, .T. ) ;
#17611 = CARTESIAN_POINT ( 'NONE',  ( 97.71630809606563162, 241.5330865364753095, 11.29444388666043331 ) ) ;
#17612 = B_SPLINE_CURVE_WITH_KNOTS ( 'NONE', 3,
 ( #26, #4604, #6485, #19702, #15267, #19984, #24022, #8784, #4327, #6633, #17542, #15691, #26303, #13117, #15408, #24163, #13250, #21997, #13390, #2449, #22142, #2304, #21571, #17830, #21719, #11086, #19843, #8930, #1884, #10662, #166, #17689, #26437, #6765, #15546, #24295, #19420, #11234, #28167, #9072, #2032, #26583, #8507, #26018 ),
 .UNSPECIFIED., .F., .F.,
 ( 4, 2, 2, 2, 2, 2, 2, 2, 2, 2, 2, 2, 2, 2, 2, 2, 2, 2, 2, 2, 2, 4 ),
 ( 2.775557561562891351E-17, 0.001175389346958584033, 0.001763084020437862172, 0.002350778693917140311, 0.003526168040875716971, 0.004701557387834292764, 0.005876946734792868991, 0.007052336081751445218, 0.007640030755230769327, 0.008227725428710095171, 0.009403114775668663591, 0.01057850412262723375, 0.01175389346958580217, 0.01234158814306504995, 0.01292928281654429599, 0.01410467216350275860, 0.01528006151046121947, 0.01586775618394042908, 0.01645545085741964217, 0.01763084020437801977, 0.01821853487785717735, 0.01880622955133633145 ),
 .UNSPECIFIED. ) ;
#17613 = EDGE_CURVE ( 'NONE', #9726, #10441, #13184, .T. ) ;
#17614 = LINE ( 'NONE', #26649, #24083 ) ;
#17615 = DIRECTION ( 'NONE',  ( 0.000000000000000000, 0.000000000000000000, -1.000000000000000000 ) ) ;
#17616 = VECTOR ( 'NONE', #13419, 1000.000000000000000 ) ;
#17617 = CARTESIAN_POINT ( 'NONE',  ( 116.5224093497741364, 227.6536686473013447, -45.00000000000000000 ) ) ;
#17618 = CARTESIAN_POINT ( 'NONE',  ( 157.9999999999996589, 273.6653751576470768, 45.00000000000000000 ) ) ;
#17619 = DIRECTION ( 'NONE',  ( 0.8916010070293384215, 0.4528218681383106015, 0.000000000000000000 ) ) ;
#17620 = PRODUCT_DEFINITION_SHAPE ( 'NONE', 'NONE',  #8432 ) ;
#17621 = DIRECTION ( 'NONE',  ( 1.000000000000000000, -0.000000000000000000, -0.000000000000000000 ) ) ;
#17622 = B_SPLINE_CURVE_WITH_KNOTS ( 'NONE', 3,
 ( #17012, #5534, #16741, #3513, #21039, #19030 ),
 .UNSPECIFIED., .F., .F.,
 ( 4, 2, 4 ),
 ( 0.000000000000000000, 0.004615224477119856880, 0.009230448954239713760 ),
 .UNSPECIFIED. ) ;
#17623 = CARTESIAN_POINT ( 'NONE',  ( -272.1612352632698162, -170.1778405466225763, -92.98998843785479096 ) ) ;
#17624 = ADVANCED_FACE ( 'NONE', ( #11020 ), #24226, .F. ) ;
#17625 = VECTOR ( 'NONE', #28173, 1000.000000000000000 ) ;
#17626 = LINE ( 'NONE', #24520, #5566 ) ;
#17627 = LINE ( 'NONE', #23673, #1744 ) ;
#17628 = CARTESIAN_POINT ( 'NONE',  ( 162.6509609271901411, 34.34969631929494938, 45.00000000000000000 ) ) ;
#17629 = ORIENTED_EDGE ( 'NONE', *, *, #27755, .F. ) ;
#17630 = DIRECTION ( 'NONE',  ( 0.000000000000000000, -1.000000000000000000, -1.214306433183764966E-16 ) ) ;
#17631 = DIRECTION ( 'NONE',  ( -1.000000000000000000, -2.602085213965211135E-16, -0.000000000000000000 ) ) ;
#17632 = CARTESIAN_POINT ( 'NONE',  ( 232.4999999999996305, 83.06687458711267880, 36.86484227207694175 ) ) ;
#17633 = CARTESIAN_POINT ( 'NONE',  ( 0.1707501505551958787, -1.250000000000000444, 7.345390377919865266 ) ) ;
#17634 = VERTEX_POINT ( 'NONE', #9289 ) ;
#17635 = EDGE_CURVE ( 'NONE', #20120, #9545, #5994, .T. ) ;
#17636 = CARTESIAN_POINT ( 'NONE',  ( 158.0000000000001990, 186.3976249024084666, -45.00000000000000000 ) ) ;
#17637 = EDGE_LOOP ( 'NONE', ( #19482, #13598, #6580, #11838 ) ) ;
#17638 = FACE_OUTER_BOUND ( 'NONE', #6809, .T. ) ;
#17639 = VERTEX_POINT ( 'NONE', #26371 ) ;
#17640 = CIRCLE ( 'NONE', #23137, 35.18636678425507114 ) ;
#17641 = ORIENTED_EDGE ( 'NONE', *, *, #16758, .T. ) ;
#17642 = ORIENTED_EDGE ( 'NONE', *, *, #15960, .F. ) ;
#17643 = VECTOR ( 'NONE', #26103, 1000.000000000000000 ) ;
#17644 = ORIENTED_EDGE ( 'NONE', *, *, #602, .T. ) ;
#17645 = VERTEX_POINT ( 'NONE', #26088 ) ;
#17646 = LINE ( 'NONE', #24542, #12754 ) ;
#17647 = DIRECTION ( 'NONE',  ( 1.000000000000000000, -0.000000000000000000, -0.000000000000000000 ) ) ;
#17648 = EDGE_CURVE ( 'NONE', #3887, #9114, #96, .T. ) ;
#17649 = LINE ( 'NONE', #22104, #1094 ) ;
#17650 = EDGE_CURVE ( 'NONE', #17988, #22350, #8858, .T. ) ;
#17651 = CARTESIAN_POINT ( 'NONE',  ( -213.1074610084667142, 72.43174512725488512, 29.09741138160865503 ) ) ;
#17652 = DIRECTION ( 'NONE',  ( 0.000000000000000000, 0.000000000000000000, -1.000000000000000000 ) ) ;
#17653 = DIRECTION ( 'NONE',  ( 0.000000000000000000, 0.000000000000000000, 1.000000000000000000 ) ) ;
#17654 = CARTESIAN_POINT ( 'NONE',  ( 158.0000000000013927, 75.54324956459154805, 45.00000000000000000 ) ) ;
#17655 = DIRECTION ( 'NONE',  ( -0.8916010070293384215, 0.4528218681383106015, 0.000000000000000000 ) ) ;
#17656 = EDGE_CURVE ( 'NONE', #2009, #4054, #18391, .T. ) ;
#17657 = LINE ( 'NONE', #1850, #4022 ) ;
#17658 = CARTESIAN_POINT ( 'NONE',  ( -222.5035551981610240, 71.60080523241312278, -19.89305531471348942 ) ) ;
#17659 = FACE_OUTER_BOUND ( 'NONE', #6821, .T. ) ;
#17660 = CARTESIAN_POINT ( 'NONE',  ( -260.0000000000001137, -165.0000000000001137, -59.99999999999986500 ) ) ;
#17661 = CARTESIAN_POINT ( 'NONE',  ( 158.0000000000013927, 75.54324956459154805, 45.00000000000000000 ) ) ;
#17662 = DIRECTION ( 'NONE',  ( 0.8916010070298056034, 0.4528218681373908372, 0.000000000000000000 ) ) ;
#17663 = CIRCLE ( 'NONE', #5282, 35.18636678425505693 ) ;
#17665 = ORIENTED_EDGE ( 'NONE', *, *, #11774, .T. ) ;
#17664 = ORIENTED_EDGE ( 'NONE', *, *, #26599, .T. ) ;
#17666 = CARTESIAN_POINT ( 'NONE',  ( -184.0370960732481365, 107.2191430342065956, 32.03030874554431051 ) ) ;
#17667 = CARTESIAN_POINT ( 'NONE',  ( -205.2903385372944172, 91.43253450480416689, -27.40388414340571188 ) ) ;
#17668 = ORIENTED_EDGE ( 'NONE', *, *, #25864, .T. ) ;
#17669 = ORIENTED_EDGE ( 'NONE', *, *, #2047, .F. ) ;
#17670 = ORIENTED_EDGE ( 'NONE', *, *, #27551, .F. ) ;
#17672 = LINE ( 'NONE', #6324, #24889 ) ;
#17671 = B_SPLINE_CURVE_WITH_KNOTS ( 'NONE', 3,
 ( #27237, #5829, #5548, #10150, #12177, #25371, #7845, #7577, #5693, #10289, #14185, #18622, #14463, #8130, #3526, #1518, #23220, #20638 ),
 .UNSPECIFIED., .F., .F.,
 ( 4, 2, 2, 2, 2, 2, 2, 2, 4 ),
 ( 0.000000000000000000, 0.006294660581775916169, 0.009441990872663860376, 0.01101565601810783682, 0.01258932116355180979, 0.01888398174532769994, 0.02045764689077167117, 0.02203131203621564588, 0.02517864232710359182 ),
 .UNSPECIFIED. ) ;
#17673 = CARTESIAN_POINT ( 'NONE',  ( -107.9485888623679983, 135.2281170464213744, 15.33484527251397722 ) ) ;
#17674 = ORIENTED_EDGE ( 'NONE', *, *, #8652, .F. ) ;
#17675 = AXIS2_PLACEMENT_3D ( 'NONE', #20904, #1225, #18747 ) ;
#17676 = AXIS2_PLACEMENT_3D ( 'NONE', #245, #26507, #17757 ) ;
#17677 = VECTOR ( 'NONE', #15915, 1000.000000000000000 ) ;
#17678 = CARTESIAN_POINT ( 'NONE',  ( 118.4313905927012343, 122.3304618272157569, -100.0000000000000142 ) ) ;
#17679 = CARTESIAN_POINT ( 'NONE',  ( 157.4999999999998579, 85.82868709837320864, -45.00000000000000000 ) ) ;
#17680 = VERTEX_POINT ( 'NONE', #17617 ) ;
#17681 = EDGE_CURVE ( 'NONE', #1943, #5089, #23951, .T. ) ;
#17682 = CARTESIAN_POINT ( 'NONE',  ( -221.8871453966669378, 88.28839002355613275, 15.46908442505722014 ) ) ;
#17683 = CIRCLE ( 'NONE', #721, 4.999999999999992895 ) ;
#17684 = CARTESIAN_POINT ( 'NONE',  ( 209.9999999999999432, -280.0000000000000000, 99.99999999999991473 ) ) ;
#17685 = EDGE_CURVE ( 'NONE', #7854, #26801, #22053, .T. ) ;
#17686 = ADVANCED_FACE ( 'NONE', ( #17904 ), #2099, .F. ) ;
#17687 = EDGE_CURVE ( 'NONE', #5281, #28009, #22505, .T. ) ;
#17688 = CARTESIAN_POINT ( 'NONE',  ( 232.4999999999996305, 133.0668745871126930, 30.83984227207694317 ) ) ;
#17689 = CARTESIAN_POINT ( 'NONE',  ( 158.7724735843374333, 201.6983920632174829, -140.4781857268138765 ) ) ;
#17690 = VERTEX_POINT ( 'NONE', #2810 ) ;
#17691 = DIRECTION ( 'NONE',  ( 0.000000000000000000, 0.000000000000000000, -1.000000000000000000 ) ) ;
#17692 = VECTOR ( 'NONE', #16227, 1000.000000000000000 ) ;
#17693 = CARTESIAN_POINT ( 'NONE',  ( -227.8378063125350366, 130.6400894613935577, -15.00000000000000178 ) ) ;
#17694 = CARTESIAN_POINT ( 'NONE',  ( 158.0000000000000853, 200.9369999399436892, -45.00000000000000000 ) ) ;
#17695 = CARTESIAN_POINT ( 'NONE',  ( 115.6411010564591777, 208.5333949359988139, -99.00000000000001421 ) ) ;
#17696 = ORIENTED_EDGE ( 'NONE', *, *, #20800, .T. ) ;
#17697 = AXIS2_PLACEMENT_3D ( 'NONE', #7079, #11398, #18146 ) ;
#17698 = CARTESIAN_POINT ( 'NONE',  ( 157.4999999999998295, 228.7775625262745223, 45.00000000000000000 ) ) ;
#17699 = DIRECTION ( 'NONE',  ( 0.000000000000000000, 0.000000000000000000, -1.000000000000000000 ) ) ;
#17700 = CARTESIAN_POINT ( 'NONE',  ( -139.6220413667664388, 71.47158950552817203, 82.81269952352197095 ) ) ;
#17701 = ORIENTED_EDGE ( 'NONE', *, *, #7953, .T. ) ;
#17702 = VECTOR ( 'NONE', #4859, 1000.000000000000114 ) ;
#17703 = ORIENTED_EDGE ( 'NONE', *, *, #6375, .T. ) ;
#17704 = DIRECTION ( 'NONE',  ( 0.000000000000000000, 0.000000000000000000, -1.000000000000000000 ) ) ;
#17705 = CARTESIAN_POINT ( 'NONE',  ( -180.4477663358212851, 109.7449299953589303, -30.47011597699462726 ) ) ;
#17706 = ORIENTED_EDGE ( 'NONE', *, *, #16527, .T. ) ;
#17707 = ORIENTED_EDGE ( 'NONE', *, *, #5523, .F. ) ;
#17708 = PLANE ( 'NONE',  #8580 ) ;
#17709 = EDGE_CURVE ( 'NONE', #1480, #26626, #7701, .T. ) ;
#17710 = EDGE_CURVE ( 'NONE', #4413, #11964, #3232, .T. ) ;
#17711 = DIRECTION ( 'NONE',  ( -0.000000000000000000, -0.000000000000000000, -1.000000000000000000 ) ) ;
#17712 = VERTEX_POINT ( 'NONE', #24802 ) ;
#17713 = ORIENTED_EDGE ( 'NONE', *, *, #18656, .T. ) ;
#17714 = VECTOR ( 'NONE', #15331, 1000.000000000000000 ) ;
#17715 = CARTESIAN_POINT ( 'NONE',  ( 157.4999999999998579, 168.5885623461056184, -45.00000000000000000 ) ) ;
#17716 = EDGE_CURVE ( 'NONE', #19657, #4881, #7562, .T. ) ;
#17717 = EDGE_CURVE ( 'NONE', #14427, #1808, #2307, .T. ) ;
#17718 = CARTESIAN_POINT ( 'NONE',  ( 157.9999999999997726, 241.5708750675630370, -45.00000000000000000 ) ) ;
#17719 = CARTESIAN_POINT ( 'NONE',  ( 158.0000000000013358, 78.55899957960562574, 45.00000000000000000 ) ) ;
#17720 = CARTESIAN_POINT ( 'NONE',  ( 134.9999999999998579, 433.5940952139197293, -145.0000000000000000 ) ) ;
#17721 = VECTOR ( 'NONE', #17019, 1000.000000000000000 ) ;
#17722 = DIRECTION ( 'NONE',  ( 0.8916010070297846202, -0.4528218681374320265, 0.000000000000000000 ) ) ;
#17723 = CARTESIAN_POINT ( 'NONE',  ( -209.1829230853339254, 69.04436975541815968, -36.49242910384992200 ) ) ;
#17724 = CARTESIAN_POINT ( 'NONE',  ( 217.4999999999996305, 133.0668745871126930, -42.86484227207692044 ) ) ;
#17725 = EDGE_LOOP ( 'NONE', ( #15825, #18982, #17113, #24853 ) ) ;
#17726 = CARTESIAN_POINT ( 'NONE',  ( 187.4999999999996305, 258.6181251126050711, 1.387778780781445676E-14 ) ) ;
#17727 = CARTESIAN_POINT ( 'NONE',  ( -175.0000000000000000, -170.0000000000001990, -75.99999999999995737 ) ) ;
#17728 = FACE_OUTER_BOUND ( 'NONE', #7110, .T. ) ;
#17729 = CARTESIAN_POINT ( 'NONE',  ( -146.6428522700808230, 17.24192588826928585, 80.00000000000001421 ) ) ;
#17730 = ORIENTED_EDGE ( 'NONE', *, *, #14945, .T. ) ;
#17731 = CARTESIAN_POINT ( 'NONE',  ( -217.3069758534620632, 60.48634897156495782, 12.43751791598376677 ) ) ;
#17732 = ORIENTED_EDGE ( 'NONE', *, *, #16092, .F. ) ;
#17733 = CARTESIAN_POINT ( 'NONE',  ( 158.0000000000003411, 175.8582498648732440, 45.00000000000000000 ) ) ;
#17734 = CARTESIAN_POINT ( 'NONE',  ( 162.6509609271901411, 34.34969631929494938, 45.00000000000000000 ) ) ;
#17735 = CARTESIAN_POINT ( 'NONE',  ( 140.9615602964835261, 249.4018026332753095, -145.7848141779618913 ) ) ;
#17736 = ORIENTED_EDGE ( 'NONE', *, *, #21182, .F. ) ;
#17737 = SURFACE_STYLE_FILL_AREA ( #220 ) ;
#17738 = ORIENTED_EDGE ( 'NONE', *, *, #16431, .T. ) ;
#17739 = VECTOR ( 'NONE', #4625, 1000.000000000000114 ) ;
#17740 = LINE ( 'NONE', #24212, #4256 ) ;
#17741 = ORIENTED_EDGE ( 'NONE', *, *, #4838, .T. ) ;
#17742 = FACE_OUTER_BOUND ( 'NONE', #17725, .T. ) ;
#17743 = ORIENTED_EDGE ( 'NONE', *, *, #11957, .F. ) ;
#17744 = VERTEX_POINT ( 'NONE', #7277 ) ;
#17745 = DIRECTION ( 'NONE',  ( 3.469446951953614189E-16, -1.000000000000000000, 0.000000000000000000 ) ) ;
#17746 = ORIENTED_EDGE ( 'NONE', *, *, #16876, .F. ) ;
#17747 = EDGE_CURVE ( 'NONE', #15219, #11070, #18613, .T. ) ;
#17748 = ORIENTED_EDGE ( 'NONE', *, *, #15398, .T. ) ;
#17749 = EDGE_LOOP ( 'NONE', ( #13415, #18899, #25581, #5897 ) ) ;
#17750 = CARTESIAN_POINT ( 'NONE',  ( -221.1044245926502754, 138.9463871349997532, 14.97905406095742364 ) ) ;
#17751 = CARTESIAN_POINT ( 'NONE',  ( 90.84405255074190677, 240.0000000000000284, 6.597066685410527320 ) ) ;
#17752 = DIRECTION ( 'NONE',  ( -0.8916010070297338830, 0.4528218681375318910, 0.000000000000000000 ) ) ;
#17753 = LINE ( 'NONE', #4674, #2253 ) ;
#17754 = VECTOR ( 'NONE', #11401, 1000.000000000000000 ) ;
#17755 = AXIS2_PLACEMENT_3D ( 'NONE', #23976, #269, #13073 ) ;
#17756 = CARTESIAN_POINT ( 'NONE',  ( 134.9999999999998579, 220.0000000000000284, -105.0000000000000284 ) ) ;
#17757 = DIRECTION ( 'NONE',  ( -1.000000000000000000, 4.540956701092242152E-16, 0.000000000000000000 ) ) ;
#17758 = CARTESIAN_POINT ( 'NONE',  ( 39.99999999999995737, 59.99999999999980105, 110.0000000000000284 ) ) ;
#17759 = EDGE_CURVE ( 'NONE', #27097, #19656, #13903, .T. ) ;
#17760 = LINE ( 'NONE', #6422, #24133 ) ;
#17761 = LINE ( 'NONE', #26374, #2997 ) ;
#17762 = LINE ( 'NONE', #8863, #10614 ) ;
#17763 = DIRECTION ( 'NONE',  ( 0.000000000000000000, 0.000000000000000000, 1.000000000000000000 ) ) ;
#17764 = CARTESIAN_POINT ( 'NONE',  ( -201.8712871270307971, 91.53752412319903442, 28.77272332722129988 ) ) ;
#17765 = ORIENTED_EDGE ( 'NONE', *, *, #26523, .F. ) ;
#17766 = DIRECTION ( 'NONE',  ( 1.000000000000000000, 0.000000000000000000, -0.000000000000000000 ) ) ;
#17767 = DIRECTION ( 'NONE',  ( 0.4528218681382754074, -0.8916010070293562961, 0.000000000000000000 ) ) ;
#17768 = DIRECTION ( 'NONE',  ( 0.000000000000000000, -1.000000000000000000, -1.214306433183764966E-16 ) ) ;
#17769 = DIRECTION ( 'NONE',  ( -0.000000000000000000, 0.000000000000000000, 1.000000000000000000 ) ) ;
#17770 = VERTEX_POINT ( 'NONE', #24658 ) ;
#17771 = EDGE_CURVE ( 'NONE', #15393, #12920, #2957, .T. ) ;
#17772 = PLANE ( 'NONE',  #6098 ) ;
#17773 = ORIENTED_EDGE ( 'NONE', *, *, #13635, .F. ) ;
#17774 =( NAMED_UNIT ( * ) PLANE_ANGLE_UNIT ( ) SI_UNIT ( $, .RADIAN. ) );
#17775 = ORIENTED_EDGE ( 'NONE', *, *, #8287, .T. ) ;
#17776 = CIRCLE ( 'NONE', #8144, 1.000000000000000888 ) ;
#17777 = ORIENTED_EDGE ( 'NONE', *, *, #10517, .T. ) ;
#17778 = EDGE_CURVE ( 'NONE', #2965, #21780, #5536, .T. ) ;
#17779 = VERTEX_POINT ( 'NONE', #9576 ) ;
#17780 = VERTEX_POINT ( 'NONE', #27089 ) ;
#17781 = ORIENTED_EDGE ( 'NONE', *, *, #10956, .F. ) ;
#17782 = DIRECTION ( 'NONE',  ( 0.8916010070295614653, -0.4528218681378716193, 0.000000000000000000 ) ) ;
#17783 = FACE_OUTER_BOUND ( 'NONE', #27081, .T. ) ;
#17784 = DIRECTION ( 'NONE',  ( -0.9506505318133460225, 0.3102637045530823867, 0.000000000000000000 ) ) ;
#17785 = DIRECTION ( 'NONE',  ( -0.8916010070296022105, 0.4528218681377911281, 0.000000000000000000 ) ) ;
#17786 = LINE ( 'NONE', #12929, #23101 ) ;
#17787 = EDGE_CURVE ( 'NONE', #14580, #13671, #7419, .T. ) ;
#17788 = CARTESIAN_POINT ( 'NONE',  ( -200.3909388571092052, 61.22025098964192580, 27.25552298266466167 ) ) ;
#17790 = CARTESIAN_POINT ( 'NONE',  ( 157.4751130497509450, 224.9869122110685566, 45.00000000000000000 ) ) ;
#17789 = TOROIDAL_SURFACE ( 'NONE', #6773, 7.509856658345970715, 10.53396790234564762 ) ;
#17791 = PLANE ( 'NONE',  #10356 ) ;
#17792 = EDGE_CURVE ( 'NONE', #24488, #23655, #11046, .T. ) ;
#17793 = CYLINDRICAL_SURFACE ( 'NONE', #21377, 2.000000000000000000 ) ;
#17794 = AXIS2_PLACEMENT_3D ( 'NONE', #19845, #13395, #12977 ) ;
#17795 = DIRECTION ( 'NONE',  ( -0.7440215159219033536, 0.6681556583950127859, 0.000000000000000000 ) ) ;
#17796 = CARTESIAN_POINT ( 'NONE',  ( -260.0000000000001137, -165.0000000000001137, 60.00000000000002132 ) ) ;
#17797 = CARTESIAN_POINT ( 'NONE',  ( 100.5794065449870942, 118.1137289701970872, 81.24999999968734699 ) ) ;
#17798 = CARTESIAN_POINT ( 'NONE',  ( 6.407398492414470681, 140.2478795492215227, 14.93043396175051463 ) ) ;
#17799 = DIRECTION ( 'NONE',  ( 4.540956701092242152E-16, 1.000000000000000000, 0.000000000000000000 ) ) ;
#17800 = DIRECTION ( 'NONE',  ( 1.000000000000000000, -0.000000000000000000, -0.000000000000000000 ) ) ;
#17801 = LINE ( 'NONE', #21693, #12509 ) ;
#17803 = ORIENTED_EDGE ( 'NONE', *, *, #12210, .T. ) ;
#17802 = ORIENTED_EDGE ( 'NONE', *, *, #26001, .F. ) ;
#17804 = EDGE_CURVE ( 'NONE', #14369, #15187, #9714, .T. ) ;
#17805 = CARTESIAN_POINT ( 'NONE',  ( 157.4999999999996305, 286.4586876989355915, -45.00000000000000000 ) ) ;
#17806 = VECTOR ( 'NONE', #11477, 1000.000000000000000 ) ;
#17807 = DIRECTION ( 'NONE',  ( 0.000000000000000000, -1.000000000000000000, 0.000000000000000000 ) ) ;
#17808 = CARTESIAN_POINT ( 'NONE',  ( -206.1354706573135616, 90.30607007072229919, -28.11841259107378121 ) ) ;
#17809 = ORIENTED_EDGE ( 'NONE', *, *, #21387, .T. ) ;
#17810 = ORIENTED_EDGE ( 'NONE', *, *, #14673, .F. ) ;
#17811 = EDGE_CURVE ( 'NONE', #10728, #2611, #15015, .T. ) ;
#17813 = EDGE_CURVE ( 'NONE', #1568, #7082, #12725, .T. ) ;
#17812 = VERTEX_POINT ( 'NONE', #27499 ) ;
#17814 = VECTOR ( 'NONE', #8724, 1000.000000000000000 ) ;
#17815 = DIRECTION ( 'NONE',  ( -0.000000000000000000, -0.000000000000000000, 1.000000000000000000 ) ) ;
#17816 = LINE ( 'NONE', #22416, #24147 ) ;
#17817 = VECTOR ( 'NONE', #17722, 1000.000000000000114 ) ;
#17818 = VERTEX_POINT ( 'NONE', #12305 ) ;
#17819 = EDGE_CURVE ( 'NONE', #23293, #1808, #938, .T. ) ;
#17820 = ORIENTED_EDGE ( 'NONE', *, *, #3997, .F. ) ;
#17821 = B_SPLINE_CURVE_WITH_KNOTS ( 'NONE', 3,
 ( #27914, #28057, #10556, #5815, #9995, #5681, #16745, #10278 ),
 .UNSPECIFIED., .F., .F.,
 ( 4, 2, 2, 4 ),
 ( 3.103167691559091397E-17, 0.003477520733619440373, 0.005216281100429154272, 0.006955041467238867736 ),
 .UNSPECIFIED. ) ;
#17822 = CARTESIAN_POINT ( 'NONE',  ( 157.4999999999998579, 80.81293708335913095, 45.00000000000000000 ) ) ;
#17823 = DIRECTION ( 'NONE',  ( -0.000000000000000000, -0.000000000000000000, 1.000000000000000000 ) ) ;
#17824 = VERTEX_POINT ( 'NONE', #14452 ) ;
#17825 = LINE ( 'NONE', #20266, #12372 ) ;
#17826 = DIRECTION ( 'NONE',  ( 0.000000000000000000, -1.000000000000000000, 0.000000000000000000 ) ) ;
#17827 = VECTOR ( 'NONE', #23497, 1000.000000000000000 ) ;
#17828 = CARTESIAN_POINT ( 'NONE',  ( 158.0000000000007958, 130.7164997297464595, -45.00000000000000000 ) ) ;
#17829 = EDGE_CURVE ( 'NONE', #9601, #6438, #19033, .T. ) ;
#17830 = CARTESIAN_POINT ( 'NONE',  ( 157.5858673906874685, 200.2545008562565556, -143.4408232581956497 ) ) ;
#17831 = CARTESIAN_POINT ( 'NONE',  ( -211.4394172367854594, 73.16162223722503199, -31.69164223701190153 ) ) ;
#17832 = AXIS2_PLACEMENT_3D ( 'NONE', #21614, #1927, #23919 ) ;
#17833 = ORIENTED_EDGE ( 'NONE', *, *, #6270, .T. ) ;
#17834 = PLANE ( 'NONE',  #19202 ) ;
#17835 = CARTESIAN_POINT ( 'NONE',  ( -237.3870311360069536, 121.7710280244218950, -15.00000000000000000 ) ) ;
#17836 = FACE_OUTER_BOUND ( 'NONE', #1567, .T. ) ;
#17837 = CARTESIAN_POINT ( 'NONE',  ( 134.9999999999998579, -327.2004514666934369, 84.99999999999995737 ) ) ;
#17838 = VERTEX_POINT ( 'NONE', #8118 ) ;
#17839 = DIRECTION ( 'NONE',  ( -1.000000000000000000, -0.000000000000000000, -0.000000000000000000 ) ) ;
#17840 = VECTOR ( 'NONE', #27042, 1000.000000000000000 ) ;
#17841 = DIRECTION ( 'NONE',  ( 0.000000000000000000, -1.000000000000000000, 0.000000000000000000 ) ) ;
#17842 = CARTESIAN_POINT ( 'NONE',  ( -140.9823852843819623, 70.97022185206886036, 82.84077254739482044 ) ) ;
#17843 = ORIENTED_EDGE ( 'NONE', *, *, #6434, .F. ) ;
#17844 = ORIENTED_EDGE ( 'NONE', *, *, #18949, .F. ) ;
#17845 = EDGE_CURVE ( 'NONE', #11803, #2404, #16985, .T. ) ;
#17846 = EDGE_CURVE ( 'NONE', #15188, #12495, #17821, .T. ) ;
#17847 = CARTESIAN_POINT ( 'NONE',  ( 130.0130877889311591, 197.5248869502486571, 45.00000000000000000 ) ) ;
#17848 = AXIS2_PLACEMENT_3D ( 'NONE', #16718, #7951, #19710 ) ;
#17849 = FACE_OUTER_BOUND ( 'NONE', #22276, .T. ) ;
#17850 = EDGE_LOOP ( 'NONE', ( #20847, #17600, #22469, #23748 ) ) ;
#17851 = CIRCLE ( 'NONE', #8688, 67.21503689626328537 ) ;
#17852 = ORIENTED_EDGE ( 'NONE', *, *, #84, .F. ) ;
#17853 = DIRECTION ( 'NONE',  ( -0.000000000000000000, -0.000000000000000000, -1.000000000000000000 ) ) ;
#17854 = VECTOR ( 'NONE', #23534, 1000.000000000000000 ) ;
#17855 = DIRECTION ( 'NONE',  ( 1.000000000000000000, 4.163336342344337027E-16, 0.000000000000000000 ) ) ;
#17856 = ORIENTED_EDGE ( 'NONE', *, *, #15720, .F. ) ;
#17857 = VERTEX_POINT ( 'NONE', #14731 ) ;
#17858 = DIRECTION ( 'NONE',  ( 0.6140342761796236948, -0.7892793597178160425, 0.000000000000000000 ) ) ;
#17859 = VECTOR ( 'NONE', #25982, 1000.000000000000227 ) ;
#17860 = EDGE_CURVE ( 'NONE', #4420, #4251, #1368, .T. ) ;
#17861 = CARTESIAN_POINT ( 'NONE',  ( 179.9999999999999147, -150.0000000000000284, -84.99999999999997158 ) ) ;
#17862 = FACE_OUTER_BOUND ( 'NONE', #18194, .T. ) ;
#17863 = CARTESIAN_POINT ( 'NONE',  ( -28.20803558630204222, 129.1553303067010177, -16.99816387164270637 ) ) ;
#17864 = CARTESIAN_POINT ( 'NONE',  ( 157.4999999999998579, 110.9074371734436255, -45.00000000000000000 ) ) ;
#17865 = CARTESIAN_POINT ( 'NONE',  ( -274.6583047828685835, -170.0000000000001137, 102.7143168399017270 ) ) ;
#17866 = CARTESIAN_POINT ( 'NONE',  ( -66.57029700917655646, 102.2156118568357783, -45.00000000000000000 ) ) ;
#17867 = ORIENTED_EDGE ( 'NONE', *, *, #16567, .T. ) ;
#17868 = AXIS2_PLACEMENT_3D ( 'NONE', #21925, #13044, #11019 ) ;
#17869 = EDGE_CURVE ( 'NONE', #21761, #1908, #19314, .T. ) ;
#17870 = CARTESIAN_POINT ( 'NONE',  ( 157.4999999999998579, 163.5728123310915407, -45.00000000000000000 ) ) ;
#17871 = CIRCLE ( 'NONE', #5482, 10.00000000000000888 ) ;
#17872 = CARTESIAN_POINT ( 'NONE',  ( 232.4999999999996305, 83.06687458711267880, -42.86484227207692754 ) ) ;
#17873 = LINE ( 'NONE', #21401, #414 ) ;
#17874 = LINE ( 'NONE', #9113, #16252 ) ;
#17875 = ORIENTED_EDGE ( 'NONE', *, *, #24214, .F. ) ;
#17876 = DIRECTION ( 'NONE',  ( 0.000000000000000000, -1.000000000000000000, 0.000000000000000000 ) ) ;
#17877 = AXIS2_PLACEMENT_3D ( 'NONE', #2787, #13438, #9119 ) ;
#17878 = ORIENTED_EDGE ( 'NONE', *, *, #19865, .F. ) ;
#17879 = LINE ( 'NONE', #22334, #23063 ) ;
#17880 = CARTESIAN_POINT ( 'NONE',  ( -36.37721155344281243, 172.2515494757248291, 45.00000000000000000 ) ) ;
#17881 = DIRECTION ( 'NONE',  ( 0.8660254037844394848, 0.4999999999999985012, 0.000000000000000000 ) ) ;
#17882 = ORIENTED_EDGE ( 'NONE', *, *, #14133, .T. ) ;
#17883 = PLANE ( 'NONE',  #17496 ) ;
#17884 =( LENGTH_UNIT ( ) NAMED_UNIT ( * ) SI_UNIT ( .MILLI., .METRE. ) );
#17885 = EDGE_CURVE ( 'NONE', #25868, #13016, #18890, .T. ) ;
#17886 = ORIENTED_EDGE ( 'NONE', *, *, #11548, .T. ) ;
#17887 = AXIS2_PLACEMENT_3D ( 'NONE', #19910, #15766, #9000 ) ;
#17888 = EDGE_CURVE ( 'NONE', #3327, #12285, #25361, .T. ) ;
#17889 = CARTESIAN_POINT ( 'NONE',  ( -209.1748869478697088, 74.44636301937694611, 36.40700551438309418 ) ) ;
#17890 = ORIENTED_EDGE ( 'NONE', *, *, #25355, .F. ) ;
#17891 = EDGE_CURVE ( 'NONE', #16411, #5808, #23345, .T. ) ;
#17892 = DIRECTION ( 'NONE',  ( -0.000000000000000000, -0.000000000000000000, -1.000000000000000000 ) ) ;
#17893 = EDGE_LOOP ( 'NONE', ( #1447, #1802, #24707, #4907, #25539, #5246 ) ) ;
#17894 = ORIENTED_EDGE ( 'NONE', *, *, #16744, .F. ) ;
#17895 = DIRECTION ( 'NONE',  ( 1.000000000000000000, 0.000000000000000000, -0.000000000000000000 ) ) ;
#17896 = ORIENTED_EDGE ( 'NONE', *, *, #7075, .F. ) ;
#17897 = AXIS2_PLACEMENT_3D ( 'NONE', #23206, #12303, #25770 ) ;
#17898 = ORIENTED_EDGE ( 'NONE', *, *, #13555, .F. ) ;
#17899 = ORIENTED_EDGE ( 'NONE', *, *, #20281, .T. ) ;
#17900 = CARTESIAN_POINT ( 'NONE',  ( 101.0213870967743333, 236.0005211361349780, 23.58009545579637489 ) ) ;
#17901 = CIRCLE ( 'NONE', #6882, 5.000000000000000888 ) ;
#17902 = DIRECTION ( 'NONE',  ( 0.000000000000000000, 1.000000000000000000, 0.000000000000000000 ) ) ;
#17903 = CARTESIAN_POINT ( 'NONE',  ( 158.0000000000007105, 136.2401247522676044, -45.00000000000000000 ) ) ;
#17904 = FACE_OUTER_BOUND ( 'NONE', #22086, .T. ) ;
#17905 = DIRECTION ( 'NONE',  ( 1.000000000000000000, 0.000000000000000000, 0.000000000000000000 ) ) ;
#17906 = CARTESIAN_POINT ( 'NONE',  ( 32.36067977499787673, 79.99999999999998579, 100.0000000000000142 ) ) ;
#17907 = DIRECTION ( 'NONE',  ( -1.000000000000000000, 0.000000000000000000, -0.000000000000000000 ) ) ;
#17908 = DIRECTION ( 'NONE',  ( 0.000000000000000000, 0.7071067811865476838, 0.7071067811865474617 ) ) ;
#17909 = FACE_OUTER_BOUND ( 'NONE', #11089, .T. ) ;
#17910 = DIRECTION ( 'NONE',  ( 0.000000000000000000, 0.000000000000000000, 1.000000000000000000 ) ) ;
#17911 = CARTESIAN_POINT ( 'NONE',  ( 39.99999999999996447, 59.99999999999981526, 110.0000000000000284 ) ) ;
#17912 = ORIENTED_EDGE ( 'NONE', *, *, #3642, .F. ) ;
#17913 = LINE ( 'NONE', #6707, #8307 ) ;
#17914 = EDGE_CURVE ( 'NONE', #22044, #27664, #17158, .T. ) ;
#17915 = TOROIDAL_SURFACE ( 'NONE', #15632, 30.49120955644046660, 2.000000000000000000 ) ;
#17916 = CARTESIAN_POINT ( 'NONE',  ( 158.0000000000005969, 150.7794997898028271, 45.00000000000000000 ) ) ;
#17917 = CARTESIAN_POINT ( 'NONE',  ( 232.4999999999996305, 186.4134324495536248, 35.02193266779035952 ) ) ;
#17918 = DIRECTION ( 'NONE',  ( 1.000000000000000000, 9.114230653120950357E-16, 0.000000000000000000 ) ) ;
#17919 = ORIENTED_EDGE ( 'NONE', *, *, #22787, .T. ) ;
#17920 = VECTOR ( 'NONE', #2173, 1000.000000000000000 ) ;
#17921 = CARTESIAN_POINT ( 'NONE',  ( 109.1380356258695343, 251.5976846382811516, -37.70750237628016066 ) ) ;
#17922 = ORIENTED_EDGE ( 'NONE', *, *, #10548, .F. ) ;
#17923 = EDGE_CURVE ( 'NONE', #24347, #372, #23208, .T. ) ;
#17924 = CARTESIAN_POINT ( 'NONE',  ( -31.54599830503473257, 129.2273688777865175, -15.65862693969986097 ) ) ;
#17925 = ORIENTED_EDGE ( 'NONE', *, *, #54, .T. ) ;
#17926 = ORIENTED_EDGE ( 'NONE', *, *, #15714, .F. ) ;
#17927 = EDGE_CURVE ( 'NONE', #19893, #2965, #25916, .T. ) ;
#17928 = VERTEX_POINT ( 'NONE', #3514 ) ;
#17929 = ORIENTED_EDGE ( 'NONE', *, *, #3209, .T. ) ;
#17930 = VERTEX_POINT ( 'NONE', #21326 ) ;
#17931 = ORIENTED_EDGE ( 'NONE', *, *, #21386, .T. ) ;
#17932 = CARTESIAN_POINT ( 'NONE',  ( 158.0000000000007674, 131.2243747372535267, 45.00000000000000000 ) ) ;
#17933 = CARTESIAN_POINT ( 'NONE',  ( -24.92338318254762441, 127.6681916698425567, -152.9999999999999432 ) ) ;
#17934 = AXIS2_PLACEMENT_3D ( 'NONE', #20872, #18714, #12409 ) ;
#17935 = DIRECTION ( 'NONE',  ( 1.000000000000000000, 0.000000000000000000, 0.000000000000000000 ) ) ;
#17936 = CARTESIAN_POINT ( 'NONE',  ( -7.373779444602154065, 132.9034487326637475, 14.27965191563540515 ) ) ;
#17937 = ADVANCED_FACE ( 'NONE', ( #16603 ), #15177, .T. ) ;
#17938 = AXIS2_PLACEMENT_3D ( 'NONE', #12098, #20839, #5752 ) ;
#17939 = CARTESIAN_POINT ( 'NONE',  ( -225.1304350307098900, 62.42764488596254324, 8.801787756205932567 ) ) ;
#17940 = CARTESIAN_POINT ( 'NONE',  ( 157.9999999999996305, 288.7126252026890256, -45.00000000000000000 ) ) ;
#17941 = CARTESIAN_POINT ( 'NONE',  ( 158.0000000000003695, 173.3503748573662051, -45.00000000000000000 ) ) ;
#17942 = CARTESIAN_POINT ( 'NONE',  ( 158.0000000000017337, 40.94087446699997912, 45.00000000000000000 ) ) ;
#17943 = PLANE ( 'NONE',  #9411 ) ;
#17944 = CYLINDRICAL_SURFACE ( 'NONE', #11066, 5.999999999999991118 ) ;
#17945 = DIRECTION ( 'NONE',  ( 0.8660254037844432595, 0.4999999999999919509, -0.000000000000000000 ) ) ;
#17946 = CARTESIAN_POINT ( 'NONE',  ( -175.0000000000000000, -170.0000000000001705, 70.00000000000001421 ) ) ;
#17947 = EDGE_CURVE ( 'NONE', #9277, #24079, #25771, .T. ) ;
#17948 = CARTESIAN_POINT ( 'NONE',  ( 46.79174272583949090, 194.0572550123460474, 12.99999999999999822 ) ) ;
#17949 = CYLINDRICAL_SURFACE ( 'NONE', #1790, 5.999999999999991118 ) ;
#17950 = CARTESIAN_POINT ( 'NONE',  ( -175.0522400338538205, 112.5415177721608444, 28.99059681523648280 ) ) ;
#17951 = DIRECTION ( 'NONE',  ( 0.9506505318133536830, 0.3102637045530589055, -0.000000000000000000 ) ) ;
#17953 = VERTEX_POINT ( 'NONE', #12863 ) ;
#17952 = ORIENTED_EDGE ( 'NONE', *, *, #111, .T. ) ;
#17954 = LINE ( 'NONE', #18105, #22923 ) ;
#17955 = VECTOR ( 'NONE', #23491, 1000.000000000000114 ) ;
#17956 = CARTESIAN_POINT ( 'NONE',  ( 151.9705627484771355, 204.4436508138959141, 45.00000000000000000 ) ) ;
#17957 = DIRECTION ( 'NONE',  ( 0.000000000000000000, -1.000000000000000000, 0.000000000000000000 ) ) ;
#17958 = VERTEX_POINT ( 'NONE', #21607 ) ;
#17959 = VERTEX_POINT ( 'NONE', #4221 ) ;
#17960 = AXIS2_PLACEMENT_3D ( 'NONE', #507, #4941, #18457 ) ;
#17961 = VERTEX_POINT ( 'NONE', #22179 ) ;
#17962 = VECTOR ( 'NONE', #15815, 1000.000000000000000 ) ;
#17963 = ADVANCED_FACE ( 'NONE', ( #10702 ), #19598, .F. ) ;
#17964 = CARTESIAN_POINT ( 'NONE',  ( 9.999999999999749534, 90.00000000000001421, 80.00000000000001421 ) ) ;
#17965 = ADVANCED_FACE ( 'NONE', ( #8683 ), #2483, .F. ) ;
#17966 = CARTESIAN_POINT ( 'NONE',  ( -142.5060805677055384, 127.4527374505125010, 16.43452876723708300 ) ) ;
#17967 = ORIENTED_EDGE ( 'NONE', *, *, #4979, .T. ) ;
#17968 = VERTEX_POINT ( 'NONE', #8547 ) ;
#17969 = LINE ( 'NONE', #16112, #15480 ) ;
#17970 = DIRECTION ( 'NONE',  ( 0.000000000000000000, -1.000000000000000000, 0.000000000000000000 ) ) ;
#17971 = ORIENTED_EDGE ( 'NONE', *, *, #11146, .F. ) ;
#17972 = CARTESIAN_POINT ( 'NONE',  ( -203.8339836453408509, 92.04912517899440161, 29.52897491471929570 ) ) ;
#17973 = CARTESIAN_POINT ( 'NONE',  ( -210.0000000000000568, -220.0000000000000853, 109.1217062362809145 ) ) ;
#17974 = EDGE_CURVE ( 'NONE', #20507, #12401, #10840, .T. ) ;
#17975 = EDGE_CURVE ( 'NONE', #13270, #21808, #23911, .T. ) ;
#17976 = AXIS2_PLACEMENT_3D ( 'NONE', #8089, #3767, #8370 ) ;
#17977 = DIRECTION ( 'NONE',  ( 1.000000000000000000, -0.000000000000000000, -0.000000000000000000 ) ) ;
#17978 = CIRCLE ( 'NONE', #9271, 9.999999999999994671 ) ;
#17979 = CARTESIAN_POINT ( 'NONE',  ( -189.8086322075389774, 92.49158130768422836, 12.99999999999999822 ) ) ;
#17980 = CARTESIAN_POINT ( 'NONE',  ( -208.5235512171359176, 74.87362916051154116, -38.25286048366049840 ) ) ;
#17981 = AXIS2_PLACEMENT_3D ( 'NONE', #7259, #18179, #9560 ) ;
#17982 = VERTEX_POINT ( 'NONE', #349 ) ;
#17983 = CARTESIAN_POINT ( 'NONE',  ( 134.9999999999998579, 220.0000000000000284, -99.00000000000001421 ) ) ;
#17984 = EDGE_CURVE ( 'NONE', #15093, #11335, #27532, .T. ) ;
#17985 = CARTESIAN_POINT ( 'NONE',  ( 158.0000000000005400, 156.3031248123239436, 45.00000000000000000 ) ) ;
#17986 = CARTESIAN_POINT ( 'NONE',  ( 112.4999999999998863, 220.0000000000000284, 99.00000000000001421 ) ) ;
#17987 = CARTESIAN_POINT ( 'NONE',  ( 134.9999999999998579, 330.0000000000000000, 84.99999999999995737 ) ) ;
#17988 = VERTEX_POINT ( 'NONE', #13286 ) ;
#17989 = CARTESIAN_POINT ( 'NONE',  ( 232.4749999999995964, 83.06687458711267880, -30.86484227207694886 ) ) ;
#17990 = CARTESIAN_POINT ( 'NONE',  ( -260.0000000000001137, -157.0000000000000284, -89.99999999999985789 ) ) ;
#17991 = CARTESIAN_POINT ( 'NONE',  ( -115.3221550338875687, 66.54464929955099706, 83.00000000000001421 ) ) ;
#17992 = ORIENTED_EDGE ( 'NONE', *, *, #5776, .T. ) ;
#17993 = CARTESIAN_POINT ( 'NONE',  ( 0.000000000000000000, 0.000000000000000000, 0.000000000000000000 ) ) ;
#17994 =( BOUNDED_SURFACE ( )  B_SPLINE_SURFACE ( 2, 3, ( 
 ( #14119, #5478, #9665, #11828, #24749, #7367, #14260, #20289, #11549, #3176, #13990, #15858, #23007, #24604, #9524, #4909, #13700, #18420, #1031, #27173, #621, #2907 ),
 ( #20569, #18282, #7510, #9384, #16134, #5343, #22870, #11966, #9803, #5763, #3739, #16691, #20988, #1448, #17109, #12813, #21273, #16828, #25442, #21555, #1866, #6188 ),
 ( #23152, #12676, #25865, #10223, #1728, #4023, #3597, #14536, #23716, #8203, #19260, #12250, #27581, #1311, #10082, #19119, #23291, #21413, #25301, #12392, #28006, #12530 ) ),
 .UNSPECIFIED., .F., .F., .F. ) 
 B_SPLINE_SURFACE_WITH_KNOTS ( ( 3, 3 ),
 ( 4, 2, 2, 2, 2, 2, 2, 2, 2, 2, 4 ),
 ( 0.000000000000000000, 1.000000000000000000 ),
 ( -0.000000000000000000, 0.009354143466934852422, 0.01870828693386970484, 0.02806243040080455553, 0.03741657386773940969, 0.04677071733467426384, 0.05612486080160911106, 0.06080193253507654161, 0.06547900426854397216, 0.07015607600201140270, 0.07483314773547881937 ),
 .UNSPECIFIED. ) 
 GEOMETRIC_REPRESENTATION_ITEM ( )  RATIONAL_B_SPLINE_SURFACE ( (
 ( 1.000000000000000000, 1.000000000000000000, 1.000000000000000000, 1.000000000000000000, 1.000000000000000000, 1.000000000000000000, 1.000000000000000000, 1.000000000000000000, 1.000000000000000000, 1.000000000000000000, 1.000000000000000000, 1.000000000000000000, 1.000000000000000000, 1.000000000000000000, 1.000000000000000000, 1.000000000000000000, 1.000000000000000000, 1.000000000000000000, 1.000000000000000000, 1.000000000000000000, 1.000000000000000000, 1.000000000000000000),
 ( 0.7071067811865480168, 0.7071067811865480168, 0.7071067811865475727, 0.7071067811865475727, 0.7071067811865475727, 0.7071067811865475727, 0.7071067811865475727, 0.7071067811865475727, 0.7071067811865475727, 0.7071067811865475727, 0.7071067811865475727, 0.7071067811865475727, 0.7071067811865475727, 0.7071067811865475727, 0.7071067811865475727, 0.7071067811865475727, 0.7071067811865475727, 0.7071067811865475727, 0.7071067811865475727, 0.7071067811865475727, 0.7071067811865475727, 0.7071067811865475727),
 ( 1.000000000000000000, 1.000000000000000000, 1.000000000000000000, 1.000000000000000000, 1.000000000000000000, 1.000000000000000000, 1.000000000000000000, 1.000000000000000000, 1.000000000000000000, 1.000000000000000000, 1.000000000000000000, 1.000000000000000000, 1.000000000000000000, 1.000000000000000000, 1.000000000000000000, 1.000000000000000000, 1.000000000000000000, 1.000000000000000000, 1.000000000000000000, 1.000000000000000000, 1.000000000000000000, 1.000000000000000000) ) ) 
 REPRESENTATION_ITEM ( '' )  SURFACE ( )  );
#17995 = ORIENTED_EDGE ( 'NONE', *, *, #22962, .T. ) ;
#17996 = AXIS2_PLACEMENT_3D ( 'NONE', #13978, #11953, #5043 ) ;
#17997 = CARTESIAN_POINT ( 'NONE',  ( -210.0000000000000000, -150.0000000000002558, -100.0000000000000142 ) ) ;
#17998 = DIRECTION ( 'NONE',  ( -0.000000000000000000, -0.000000000000000000, -1.000000000000000000 ) ) ;
#17999 = EDGE_LOOP ( 'NONE', ( #28087, #23048, #3786, #1704 ) ) ;
#18000 = CIRCLE ( 'NONE', #20292, 22.49999999999997868 ) ;
#18001 = EDGE_CURVE ( 'NONE', #1788, #761, #9725, .T. ) ;
#18002 = ORIENTED_EDGE ( 'NONE', *, *, #10927, .F. ) ;
#18003 = DIRECTION ( 'NONE',  ( -0.8660254037844362651, 0.5000000000000039968, -0.000000000000000000 ) ) ;
#18004 = VECTOR ( 'NONE', #5442, 1000.000000000000000 ) ;
#18005 = CARTESIAN_POINT ( 'NONE',  ( 158.0000000000015348, 58.49599951954928656, 45.00000000000000000 ) ) ;
#18006 = EDGE_LOOP ( 'NONE', ( #4048, #26078, #20887, #22352 ) ) ;
#18007 = PLANE ( 'NONE',  #14196 ) ;
#18008 = EDGE_LOOP ( 'NONE', ( #6548, #11859, #21752, #3355 ) ) ;
#18009 = CARTESIAN_POINT ( 'NONE',  ( -20.17488871844202691, 128.4067172797072089, 17.32976398448045430 ) ) ;
#18010 = CARTESIAN_POINT ( 'NONE',  ( 372.9108539694884144, 19.41075299063184900, 80.49671038392669686 ) ) ;
#18011 = LINE ( 'NONE', #22319, #4308 ) ;
#18012 = CARTESIAN_POINT ( 'NONE',  ( -11.10379413178596408, 130.1809569171891212, -16.64347988244048437 ) ) ;
#18013 = CARTESIAN_POINT ( 'NONE',  ( 294.9233831825460470, 127.6681916698403398, -151.0000000000000284 ) ) ;
#18014 = VECTOR ( 'NONE', #9469, 1000.000000000000000 ) ;
#18015 = EDGE_CURVE ( 'NONE', #11276, #1877, #22516, .T. ) ;
#18016 = CARTESIAN_POINT ( 'NONE',  ( -175.0000000000000000, -120.0000000000001705, 70.00000000000001421 ) ) ;
#18017 = CARTESIAN_POINT ( 'NONE',  ( 158.0000000000000568, 203.4448749474510407, -45.00000000000000000 ) ) ;
#18018 = EDGE_LOOP ( 'NONE', ( #23587, #25947, #10469, #24000 ) ) ;
#18019 = CIRCLE ( 'NONE', #23532, 10.00000000000000888 ) ;
#18020 = FACE_BOUND ( 'NONE', #23574, .T. ) ;
#18021 = DIRECTION ( 'NONE',  ( 0.000000000000000000, 0.000000000000000000, 1.000000000000000000 ) ) ;
#18022 = DIRECTION ( 'NONE',  ( -1.000000000000000000, 0.000000000000000000, 0.000000000000000000 ) ) ;
#18023 = DIRECTION ( 'NONE',  ( -0.000000000000000000, -0.000000000000000000, -1.000000000000000000 ) ) ;
#18024 = ORIENTED_EDGE ( 'NONE', *, *, #8179, .F. ) ;
#18025 = CARTESIAN_POINT ( 'NONE',  ( 158.0000000000009663, 111.1613746771971876, 45.00000000000000000 ) ) ;
#18026 = AXIS2_PLACEMENT_3D ( 'NONE', #3672, #19050, #25933 ) ;
#18027 = ORIENTED_EDGE ( 'NONE', *, *, #24162, .F. ) ;
#18028 = DIRECTION ( 'NONE',  ( -0.000000000000000000, 1.000000000000000000, -1.387778780781445429E-16 ) ) ;
#18029 = DIRECTION ( 'NONE',  ( -0.000000000000000000, -0.000000000000000000, -1.000000000000000000 ) ) ;
#18030 = CARTESIAN_POINT ( 'NONE',  ( 204.8742559748123426, 133.4291290931197977, -45.00000000000000000 ) ) ;
#18031 = VERTEX_POINT ( 'NONE', #26196 ) ;
#18032 = DIRECTION ( 'NONE',  ( -0.000000000000000000, -1.000000000000000000, -0.000000000000000000 ) ) ;
#18033 = CARTESIAN_POINT ( 'NONE',  ( 0.000000000000000000, 0.000000000000000000, 100.0000000000000142 ) ) ;
#18034 = EDGE_LOOP ( 'NONE', ( #17929, #1137, #24443, #21210 ) ) ;
#18035 = CARTESIAN_POINT ( 'NONE',  ( -222.5164088840957106, 71.60334314582038928, 19.88449668098547818 ) ) ;
#18036 = ORIENTED_EDGE ( 'NONE', *, *, #27229, .F. ) ;
#18037 = CARTESIAN_POINT ( 'NONE',  ( 158.0000000000011937, 91.09837461714084839, -45.00000000000000000 ) ) ;
#18038 = ORIENTED_EDGE ( 'NONE', *, *, #10351, .T. ) ;
#18039 = VECTOR ( 'NONE', #9535, 1000.000000000000114 ) ;
#18040 = ORIENTED_EDGE ( 'NONE', *, *, #27241, .T. ) ;
#18041 = CARTESIAN_POINT ( 'NONE',  ( 158.0000000000012506, 88.08262460212675649, -45.00000000000000000 ) ) ;
#18042 = ORIENTED_EDGE ( 'NONE', *, *, #10579, .T. ) ;
#18043 = VECTOR ( 'NONE', #16026, 1000.000000000000000 ) ;
#18044 = EDGE_CURVE ( 'NONE', #26678, #10678, #18827, .T. ) ;
#18045 = ORIENTED_EDGE ( 'NONE', *, *, #25057, .F. ) ;
#18046 = ORIENTED_EDGE ( 'NONE', *, *, #9711, .F. ) ;
#18047 = CIRCLE ( 'NONE', #17577, 5.000000000000004441 ) ;
#18048 = CARTESIAN_POINT ( 'NONE',  ( 87.49999999999990052, 230.0000000000000000, 15.95262490344436657 ) ) ;
#18049 = CARTESIAN_POINT ( 'NONE',  ( -12.24491960465745599, -23.01420295945612082, 95.00000000000000000 ) ) ;
#18050 = EDGE_CURVE ( 'NONE', #8166, #7477, #6521, .T. ) ;
#18051 = DIRECTION ( 'NONE',  ( 0.000000000000000000, 0.000000000000000000, 1.000000000000000000 ) ) ;
#18052 = EDGE_CURVE ( 'NONE', #3368, #25077, #26720, .T. ) ;
#18053 = EDGE_CURVE ( 'NONE', #26626, #14606, #26337, .T. ) ;
#18054 = CARTESIAN_POINT ( 'NONE',  ( 158.0000000000006537, 141.2558747672816821, -45.00000000000000000 ) ) ;
#18055 = LINE ( 'NONE', #20908, #25047 ) ;
#18056 = DIRECTION ( 'NONE',  ( 1.000000000000000000, 3.469446951953616161E-16, 0.000000000000000000 ) ) ;
#18057 = EDGE_CURVE ( 'NONE', #5833, #14725, #22966, .T. ) ;
#18058 = CARTESIAN_POINT ( 'NONE',  ( 157.4999999999998579, 201.1909374436971802, -45.00000000000000000 ) ) ;
#18059 = CARTESIAN_POINT ( 'NONE',  ( 5.999999999999998224, 0.000000000000000000, 0.000000000000000000 ) ) ;
#18060 = DIRECTION ( 'NONE',  ( 0.000000000000000000, -1.000000000000000000, 0.000000000000000000 ) ) ;
#18061 = DIRECTION ( 'NONE',  ( 0.8314772792026879911, -0.5555587585212703461, 0.000000000000000000 ) ) ;
#18062 = CARTESIAN_POINT ( 'NONE',  ( 52.57751368840760620, 248.9624084326366358, 45.00000000000000000 ) ) ;
#18063 = ORIENTED_EDGE ( 'NONE', *, *, #27019, .T. ) ;
#18064 = AXIS2_PLACEMENT_3D ( 'NONE', #13246, #21717, #11082 ) ;
#18065 = LINE ( 'NONE', #537, #36 ) ;
#18066 = VECTOR ( 'NONE', #6789, 1000.000000000000000 ) ;
#18067 = CARTESIAN_POINT ( 'NONE',  ( 51.56615429303207065, 203.2034914284457159, 12.99999999999999822 ) ) ;
#18068 = CYLINDRICAL_SURFACE ( 'NONE', #11701, 30.00000000000000000 ) ;
#18069 = CARTESIAN_POINT ( 'NONE',  ( 0.3651377029009472142, -1.250000000000000444, 7.402212548643258394 ) ) ;
#18070 = AXIS2_PLACEMENT_3D ( 'NONE', #12137, #11852, #9687 ) ;
#18071 = ORIENTED_EDGE ( 'NONE', *, *, #10004, .T. ) ;
#18072 = CARTESIAN_POINT ( 'NONE',  ( 109.8202728674371258, 257.1791079646811795, -41.57776855483199085 ) ) ;
#18073 = ORIENTED_EDGE ( 'NONE', *, *, #2936, .F. ) ;
#18074 = PLANE ( 'NONE',  #8171 ) ;
#18075 = ORIENTED_EDGE ( 'NONE', *, *, #8817, .T. ) ;
#18076 = VERTEX_POINT ( 'NONE', #22890 ) ;
#18077 = VERTEX_POINT ( 'NONE', #25181 ) ;
#18078 = ORIENTED_EDGE ( 'NONE', *, *, #6111, .F. ) ;
#18079 = CARTESIAN_POINT ( 'NONE',  ( -40.40953891503691153, 36.92584315232891612, 100.0000000000000000 ) ) ;
#18080 = CIRCLE ( 'NONE', #27693, 5.999999999999977796 ) ;
#18081 = LINE ( 'NONE', #20372, #24678 ) ;
#18082 = CARTESIAN_POINT ( 'NONE',  ( -175.0000000000000000, -120.0000000000001705, 63.97500000000001563 ) ) ;
#18083 = EDGE_CURVE ( 'NONE', #14664, #21625, #14006, .T. ) ;
#18084 = EDGE_CURVE ( 'NONE', #27485, #22044, #18441, .T. ) ;
#18085 = CARTESIAN_POINT ( 'NONE',  ( -97.85341642296334896, 136.0957921829576378, -13.54851073784648641 ) ) ;
#18086 = VECTOR ( 'NONE', #26443, 1000.000000000000000 ) ;
#18087 = PRODUCT_DEFINITION_CONTEXT ( 'detailed design', #2117, 'design' ) ;
#18088 = CARTESIAN_POINT ( 'NONE',  ( -175.0000000000000000, -120.0000000000001705, 70.00000000000001421 ) ) ;
#18089 = CARTESIAN_POINT ( 'NONE',  ( -224.3698807949987497, 62.17069777284014975, 9.096889663469543308 ) ) ;
#18090 = CARTESIAN_POINT ( 'NONE',  ( 114.5814157129579058, 230.6339745962151540, 45.00000000000000000 ) ) ;
#18091 = LINE ( 'NONE', #13357, #19072 ) ;
#18092 = EDGE_CURVE ( 'NONE', #9020, #7037, #5360, .T. ) ;
#18093 = LINE ( 'NONE', #423, #5766 ) ;
#18094 = PLANE ( 'NONE',  #12638 ) ;
#18095 = DIRECTION ( 'NONE',  ( 0.000000000000000000, -1.000000000000000000, 0.000000000000000000 ) ) ;
#18096 = DIRECTION ( 'NONE',  ( -0.8916010070297244461, -0.4528218681375507093, 0.000000000000000000 ) ) ;
#18097 = DIRECTION ( 'NONE',  ( -1.000000000000000000, -0.000000000000000000, -0.000000000000000000 ) ) ;
#18098 = CARTESIAN_POINT ( 'NONE',  ( -18.00535683072674686, 129.9863796852737892, 16.68487424884472858 ) ) ;
#18099 = CARTESIAN_POINT ( 'NONE',  ( -10.78991826960876033, 200.8449754580304898, 45.00000000000000000 ) ) ;
#18100 = PLANE ( 'NONE',  #23448 ) ;
#18101 = CARTESIAN_POINT ( 'NONE',  ( -260.0000000000001137, -157.0000000000000284, 95.00000000000001421 ) ) ;
#18103 = ORIENTED_EDGE ( 'NONE', *, *, #24536, .F. ) ;
#18102 = VERTEX_POINT ( 'NONE', #26776 ) ;
#18104 = VECTOR ( 'NONE', #26733, 1000.000000000000000 ) ;
#18105 = CARTESIAN_POINT ( 'NONE',  ( 157.4999999999998579, 105.8916871584295478, 45.00000000000000000 ) ) ;
#18106 = LINE ( 'NONE', #13515, #14363 ) ;
#18107 = VERTEX_POINT ( 'NONE', #20305 ) ;
#18108 = CIRCLE ( 'NONE', #13535, 1.999999999999989564 ) ;
#18109 = VERTEX_POINT ( 'NONE', #22614 ) ;
#18110 = EDGE_LOOP ( 'NONE', ( #22634, #15109, #18862, #22571, #1206, #3821, #11243, #8231, #589, #12880, #19619, #4416, #25802, #6371, #1689, #2874, #4845 ) ) ;
#18111 = DIRECTION ( 'NONE',  ( -0.000000000000000000, -0.000000000000000000, -1.000000000000000000 ) ) ;
#18112 = CARTESIAN_POINT ( 'NONE',  ( -122.9556538161509991, 132.7591345059635728, 14.33728725145604699 ) ) ;
#18113 = ORIENTED_EDGE ( 'NONE', *, *, #1880, .F. ) ;
#18114 = ORIENTED_EDGE ( 'NONE', *, *, #1539, .F. ) ;
#18115 = DIRECTION ( 'NONE',  ( -0.000000000000000000, -0.000000000000000000, -1.000000000000000000 ) ) ;
#18116 = CARTESIAN_POINT ( 'NONE',  ( 79.99999999999990052, 240.0000000000000284, -45.00000000000000000 ) ) ;
#18117 = EDGE_CURVE ( 'NONE', #14502, #21206, #7095, .T. ) ;
#18118 = DIRECTION ( 'NONE',  ( 1.000000000000000000, 0.000000000000000000, 0.000000000000000000 ) ) ;
#18119 = EDGE_LOOP ( 'NONE', ( #16184, #7848, #1477, #19831 ) ) ;
#18120 = FILL_AREA_STYLE_COLOUR ( '', #15115 ) ;
#18121 = AXIS2_PLACEMENT_3D ( 'NONE', #11948, #25141, #24729 ) ;
#18122 = CARTESIAN_POINT ( 'NONE',  ( 167.4999999999996589, 258.6181251126050711, -5.999999999999991118 ) ) ;
#18123 = LINE ( 'NONE', #7767, #4342 ) ;
#18124 = VECTOR ( 'NONE', #15457, 999.9999999999998863 ) ;
#18125 = CARTESIAN_POINT ( 'NONE',  ( 119.9999999999999432, 2.220446049250311819E-14, 90.00000000000002842 ) ) ;
#18126 = CARTESIAN_POINT ( 'NONE',  ( -212.5256769160680221, 72.66764018259178215, -29.94823517518663536 ) ) ;
#18127 = ORIENTED_EDGE ( 'NONE', *, *, #7624, .F. ) ;
#18128 = EDGE_CURVE ( 'NONE', #24580, #7480, #15876, .T. ) ;
#18129 = ADVANCED_FACE ( 'NONE', ( #22323 ), #17915, .T. ) ;
#18130 = DIRECTION ( 'NONE',  ( -0.000000000000000000, 0.000000000000000000, -1.000000000000000000 ) ) ;
#18131 = DIRECTION ( 'NONE',  ( 0.000000000000000000, 0.000000000000000000, -1.000000000000000000 ) ) ;
#18132 = CARTESIAN_POINT ( 'NONE',  ( 158.7404207507997853, 42.53436754635193040, 45.00000000000000000 ) ) ;
#18133 = DIRECTION ( 'NONE',  ( -0.000000000000000000, -0.000000000000000000, -1.000000000000000000 ) ) ;
#18134 = VERTEX_POINT ( 'NONE', #3058 ) ;
#18135 = CARTESIAN_POINT ( 'NONE',  ( 167.4999999999996589, 258.6181251126050711, 1.387778780781445676E-14 ) ) ;
#18136 = DIRECTION ( 'NONE',  ( -0.000000000000000000, -0.000000000000000000, 1.000000000000000000 ) ) ;
#18137 = DIRECTION ( 'NONE',  ( -0.2588190451024993122, 0.9659258262890740854, 0.000000000000000000 ) ) ;
#18138 = ORIENTED_EDGE ( 'NONE', *, *, #5237, .T. ) ;
#18139 = SHAPE_REPRESENTATION_RELATIONSHIP ( 'NONE' , 'NONE' ,  #22013, #5057 ) ;
#18140 = AXIS2_PLACEMENT_3D ( 'NONE', #2665, #11880, #669 ) ;
#18141 = ORIENTED_EDGE ( 'NONE', *, *, #27794, .F. ) ;
#18142 = TOROIDAL_SURFACE ( 'NONE', #24111, 39.99999999999999289, 9.999999999999996447 ) ;
#18143 = EDGE_CURVE ( 'NONE', #25694, #27854, #26917, .T. ) ;
#18144 = EDGE_CURVE ( 'NONE', #28076, #16964, #7666, .T. ) ;
#18145 = DIRECTION ( 'NONE',  ( 0.000000000000000000, 0.000000000000000000, -1.000000000000000000 ) ) ;
#18146 = DIRECTION ( 'NONE',  ( 0.4999999999999864553, -0.8660254037844463681, 0.000000000000000000 ) ) ;
#18147 = ORIENTED_EDGE ( 'NONE', *, *, #26969, .T. ) ;
#18148 = VECTOR ( 'NONE', #27167, 1000.000000000000000 ) ;
#18149 = ORIENTED_EDGE ( 'NONE', *, *, #22019, .T. ) ;
#18150 = LINE ( 'NONE', #7654, #2855 ) ;
#18151 = ORIENTED_EDGE ( 'NONE', *, *, #4425, .F. ) ;
#18152 = CARTESIAN_POINT ( 'NONE',  ( 93.99999999999985789, 171.5103103742661972, 84.99999999999995737 ) ) ;
#18153 = VERTEX_POINT ( 'NONE', #639 ) ;
#18154 = FACE_OUTER_BOUND ( 'NONE', #28060, .T. ) ;
#18155 = PLANE ( 'NONE',  #25026 ) ;
#18156 = VECTOR ( 'NONE', #7527, 1000.000000000000000 ) ;
#18157 = DIRECTION ( 'NONE',  ( 0.000000000000000000, 0.000000000000000000, 1.000000000000000000 ) ) ;
#18158 = CARTESIAN_POINT ( 'NONE',  ( -24.74149867490763910, 128.0498055069775774, -17.48283640895151692 ) ) ;
#18159 = AXIS2_PLACEMENT_3D ( 'NONE', #27641, #21184, #10416 ) ;
#18160 = DIRECTION ( 'NONE',  ( -0.8916010070295213863, -0.4528218681379502786, 0.000000000000000000 ) ) ;
#18161 = VECTOR ( 'NONE', #26796, 1000.000000000000114 ) ;
#18162 = EDGE_CURVE ( 'NONE', #14089, #8924, #2629, .T. ) ;
#18163 = CARTESIAN_POINT ( 'NONE',  ( -207.6200036923385426, 75.24376343244314569, -44.43030099895754148 ) ) ;
#18164 = CARTESIAN_POINT ( 'NONE',  ( 158.0000000000006253, 148.2716247822957882, 45.00000000000000000 ) ) ;
#18165 = ORIENTED_EDGE ( 'NONE', *, *, #11402, .T. ) ;
#18166 = ADVANCED_FACE ( 'NONE', ( #1052 ), #9542, .F. ) ;
#18167 = CARTESIAN_POINT ( 'NONE',  ( 134.9999999999998579, 220.0000000000000284, -169.9999999999999716 ) ) ;
#18168 = VECTOR ( 'NONE', #14414, 1000.000000000000000 ) ;
#18169 = CARTESIAN_POINT ( 'NONE',  ( -221.1044245926312328, 138.9463871349869066, 14.97905406095859604 ) ) ;
#18170 = FACE_OUTER_BOUND ( 'NONE', #27719, .T. ) ;
#18171 = FACE_OUTER_BOUND ( 'NONE', #21388, .T. ) ;
#18172 = ORIENTED_EDGE ( 'NONE', *, *, #13682, .F. ) ;
#18173 = CYLINDRICAL_SURFACE ( 'NONE', #16488, 2.000000000000005329 ) ;
#18174 = ORIENTED_EDGE ( 'NONE', *, *, #10219, .T. ) ;
#18175 = LINE ( 'NONE', #27205, #14847 ) ;
#18176 = DIRECTION ( 'NONE',  ( -0.8916010070298563406, -0.4528218681372909171, 0.000000000000000000 ) ) ;
#18177 = CARTESIAN_POINT ( 'NONE',  ( 137.4797360180455144, 249.8978926453951885, -139.5328759577092228 ) ) ;
#18178 = ORIENTED_EDGE ( 'NONE', *, *, #1268, .T. ) ;
#18179 = DIRECTION ( 'NONE',  ( 0.4528218681382856770, 0.8916010070293511891, -0.000000000000000000 ) ) ;
#18180 = ORIENTED_EDGE ( 'NONE', *, *, #16500, .T. ) ;
#18181 = EDGE_CURVE ( 'NONE', #5063, #24246, #5546, .T. ) ;
#18182 = DIRECTION ( 'NONE',  ( 0.4528218681382319422, 0.8916010070293783896, -0.000000000000000000 ) ) ;
#18183 = EDGE_LOOP ( 'NONE', ( #6957, #25512, #28192, #18777 ) ) ;
#18184 = LINE ( 'NONE', #18037, #5317 ) ;
#18185 = ORIENTED_EDGE ( 'NONE', *, *, #6489, .T. ) ;
#18186 = VECTOR ( 'NONE', #1122, 1000.000000000000000 ) ;
#18188 = EDGE_CURVE ( 'NONE', #16453, #23965, #5093, .T. ) ;
#18187 = VECTOR ( 'NONE', #19972, 999.9999999999998863 ) ;
#18189 = ORIENTED_EDGE ( 'NONE', *, *, #5786, .T. ) ;
#18190 = EDGE_CURVE ( 'NONE', #2723, #24747, #24907, .T. ) ;
#18191 = CARTESIAN_POINT ( 'NONE',  ( 222.4999999999996021, 186.4134324495536248, 35.02193266779035952 ) ) ;
#18192 = ORIENTED_EDGE ( 'NONE', *, *, #27072, .T. ) ;
#18193 = EDGE_CURVE ( 'NONE', #12640, #5842, #25351, .T. ) ;
#18194 = EDGE_LOOP ( 'NONE', ( #6462, #11596, #11152, #18906 ) ) ;
#18195 = AXIS2_PLACEMENT_3D ( 'NONE', #6842, #19638, #99 ) ;
#18196 = VERTEX_POINT ( 'NONE', #5644 ) ;
#18197 = CARTESIAN_POINT ( 'NONE',  ( 102.7763551498688628, 237.8836077948903096, 25.40199625706859621 ) ) ;
#18198 = DIRECTION ( 'NONE',  ( 0.000000000000000000, -1.000000000000000000, 0.000000000000000000 ) ) ;
#18199 = DIRECTION ( 'NONE',  ( 0.000000000000000000, 0.000000000000000000, 1.000000000000000000 ) ) ;
#18200 = DIRECTION ( 'NONE',  ( 0.000000000000000000, 0.000000000000000000, 1.000000000000000000 ) ) ;
#18201 = DIRECTION ( 'NONE',  ( 0.4528218681383056610, -0.8916010070293409751, 0.000000000000000000 ) ) ;
#18202 = CARTESIAN_POINT ( 'NONE',  ( 157.9999999999998295, 229.0315000300280417, 45.00000000000000000 ) ) ;
#18203 = DIRECTION ( 'NONE',  ( 0.000000000000000000, 0.000000000000000000, -1.000000000000000000 ) ) ;
#18204 = CARTESIAN_POINT ( 'NONE',  ( 157.4999999999998579, 43.19481197075347723, 45.00000000000000000 ) ) ;
#18205 = DIRECTION ( 'NONE',  ( -0.000000000000000000, -1.000000000000000000, -0.000000000000000000 ) ) ;
#18206 = CARTESIAN_POINT ( 'NONE',  ( 158.0000000000006821, 138.7479997597746433, 45.00000000000000000 ) ) ;
#18207 = CARTESIAN_POINT ( 'NONE',  ( 158.0000000000003411, 175.8582498648732440, -45.00000000000000000 ) ) ;
#18208 = VECTOR ( 'NONE', #21451, 1000.000000000000000 ) ;
#18209 = ORIENTED_EDGE ( 'NONE', *, *, #9554, .F. ) ;
#18210 = DIRECTION ( 'NONE',  ( -0.000000000000000000, 0.000000000000000000, -1.000000000000000000 ) ) ;
#18211 = CARTESIAN_POINT ( 'NONE',  ( 157.9999999999998010, 231.5393750375350237, -45.00000000000000000 ) ) ;
#18212 = DIRECTION ( 'NONE',  ( 1.000000000000000000, 0.000000000000000000, 0.000000000000000000 ) ) ;
#18213 = FACE_OUTER_BOUND ( 'NONE', #2153, .T. ) ;
#18214 = VERTEX_POINT ( 'NONE', #1743 ) ;
#18215 = CARTESIAN_POINT ( 'NONE',  ( 49.56615429303207065, 203.2034914284457159, -15.00000000000000000 ) ) ;
#18216 = EDGE_LOOP ( 'NONE', ( #9526, #18806, #22449, #18908 ) ) ;
#18217 = CARTESIAN_POINT ( 'NONE',  ( -210.0000000000000568, -160.0000000000001421, 110.0000000000000284 ) ) ;
#18218 = EDGE_CURVE ( 'NONE', #12991, #23195, #16568, .T. ) ;
#18219 = ORIENTED_EDGE ( 'NONE', *, *, #6558, .F. ) ;
#18220 = ADVANCED_FACE ( 'NONE', ( #27462 ), #3482, .F. ) ;
#18221 = ADVANCED_FACE ( 'NONE', ( #19135 ), #12550, .F. ) ;
#18222 = ORIENTED_EDGE ( 'NONE', *, *, #16649, .F. ) ;
#18223 = ORIENTED_EDGE ( 'NONE', *, *, #1722, .T. ) ;
#18224 = EDGE_LOOP ( 'NONE', ( #16379, #13780, #3571, #21878 ) ) ;
#18225 = LINE ( 'NONE', #11632, #1256 ) ;
#18226 = CIRCLE ( 'NONE', #22358, 6.000000000000005329 ) ;
#18227 = DIRECTION ( 'NONE',  ( -0.000000000000000000, 1.000000000000000000, -1.387778780781445429E-16 ) ) ;
#18228 = DIRECTION ( 'NONE',  ( 0.000000000000000000, -1.000000000000000000, 0.000000000000000000 ) ) ;
#18229 = CARTESIAN_POINT ( 'NONE',  ( -101.6720583589129063, 135.8104379926313072, -13.60266426008617913 ) ) ;
#18230 = DIRECTION ( 'NONE',  ( 1.000000000000000000, -0.000000000000000000, -0.000000000000000000 ) ) ;
#18231 = CARTESIAN_POINT ( 'NONE',  ( -213.3516035875686896, 56.48049070729076959, 40.70111258791201436 ) ) ;
#18232 = DIRECTION ( 'NONE',  ( 1.000000000000000000, 0.000000000000000000, -0.000000000000000000 ) ) ;
#18233 = CARTESIAN_POINT ( 'NONE',  ( 158.0000000000004832, 161.3188748273380213, 45.00000000000000000 ) ) ;
#18234 = CARTESIAN_POINT ( 'NONE',  ( 158.0000000000009948, 108.6534996696901345, 45.00000000000000000 ) ) ;
#18235 = CARTESIAN_POINT ( 'NONE',  ( 157.9999999999998579, 221.5078750075070104, 45.00000000000000000 ) ) ;
#18236 = FACE_OUTER_BOUND ( 'NONE', #12612, .T. ) ;
#18237 = DIRECTION ( 'NONE',  ( 0.000000000000000000, -1.000000000000000000, 0.000000000000000000 ) ) ;
#18238 = CARTESIAN_POINT ( 'NONE',  ( 98.15430812615089451, 116.0637945823775112, 78.75000000031268144 ) ) ;
#18239 = DIRECTION ( 'NONE',  ( -0.000000000000000000, 1.000000000000000000, -1.387778780781445429E-16 ) ) ;
#18240 = DIRECTION ( 'NONE',  ( 0.5150380749100565980, 1.049727191138616847E-16, 0.8571673007021108903 ) ) ;
#18241 = PLANE ( 'NONE',  #20255 ) ;
#18242 = LINE ( 'NONE', #24706, #8848 ) ;
#18244 = VERTEX_POINT ( 'NONE', #25322 ) ;
#18243 = ORIENTED_EDGE ( 'NONE', *, *, #7934, .T. ) ;
#18245 = AXIS2_PLACEMENT_3D ( 'NONE', #28124, #4141, #10619 ) ;
#18246 = CYLINDRICAL_SURFACE ( 'NONE', #5029, 10.00000000000000888 ) ;
#18247 = EDGE_CURVE ( 'NONE', #6570, #16387, #27744, .T. ) ;
#18248 = CARTESIAN_POINT ( 'NONE',  ( 157.4999999999996589, 278.9350626764145318, 45.00000000000000000 ) ) ;
#18249 = ORIENTED_EDGE ( 'NONE', *, *, #19704, .T. ) ;
#18250 = ORIENTED_EDGE ( 'NONE', *, *, #4178, .T. ) ;
#18251 = ADVANCED_FACE ( 'NONE', ( #18854 ), #10243, .F. ) ;
#18252 = FACE_OUTER_BOUND ( 'NONE', #1673, .T. ) ;
#18253 = CARTESIAN_POINT ( 'NONE',  ( -134.7028785880233102, 128.5088468861839601, 17.28571157459903773 ) ) ;
#18254 = EDGE_CURVE ( 'NONE', #12184, #12635, #1331, .T. ) ;
#18255 = ORIENTED_EDGE ( 'NONE', *, *, #25753, .T. ) ;
#18256 = ORIENTED_EDGE ( 'NONE', *, *, #16104, .F. ) ;
#18257 = LINE ( 'NONE', #7621, #26604 ) ;
#18258 = DIRECTION ( 'NONE',  ( -0.000000000000000000, 0.000000000000000000, -1.000000000000000000 ) ) ;
#18259 = VECTOR ( 'NONE', #12205, 1000.000000000000000 ) ;
#18260 = PRODUCT_RELATED_PRODUCT_CATEGORY ( 'part', '', ( #12576 ) ) ;
#18261 = FACE_OUTER_BOUND ( 'NONE', #20185, .T. ) ;
#18262 = FACE_OUTER_BOUND ( 'NONE', #10128, .T. ) ;
#18263 = CARTESIAN_POINT ( 'NONE',  ( 157.4999999999998579, 58.24206201579573872, -45.00000000000000000 ) ) ;
#18264 = CARTESIAN_POINT ( 'NONE',  ( 157.4999999999998579, 173.6043123611196961, 45.00000000000000000 ) ) ;
#18265 = PLANE ( 'NONE',  #5447 ) ;
#18266 = CARTESIAN_POINT ( 'NONE',  ( -207.7463451706791773, 75.42136631982602069, -41.72512927420302020 ) ) ;
#18267 = CARTESIAN_POINT ( 'NONE',  ( 157.9999999999997158, 261.1260001201120531, 45.00000000000000000 ) ) ;
#18268 = EDGE_CURVE ( 'NONE', #1554, #5169, #10101, .T. ) ;
#18269 = DIRECTION ( 'NONE',  ( 0.8916010070294904111, -0.4528218681380115074, 0.000000000000000000 ) ) ;
#18270 = CARTESIAN_POINT ( 'NONE',  ( -175.0000000000000000, -150.0000000000000853, -69.99999999999998579 ) ) ;
#18271 = DIRECTION ( 'NONE',  ( 0.5457381880580551847, -0.8379557447115634217, 0.000000000000000000 ) ) ;
#18272 = VERTEX_POINT ( 'NONE', #8081 ) ;
#18273 = CARTESIAN_POINT ( 'NONE',  ( 124.9999999999998579, 220.0000000000000284, -45.00000000000000000 ) ) ;
#18274 = AXIS2_PLACEMENT_3D ( 'NONE', #4719, #13503, #9187 ) ;
#18275 = ADVANCED_FACE ( 'NONE', ( #14417 ), #15650, .T. ) ;
#18276 = CARTESIAN_POINT ( 'NONE',  ( -232.3018049223844912, 76.77033509349460871, 15.55816966298073112 ) ) ;
#18277 = VECTOR ( 'NONE', #16018, 1000.000000000000000 ) ;
#18278 = DIRECTION ( 'NONE',  ( -0.9784193629480814058, -0.2066290158914539099, 0.000000000000000000 ) ) ;
#18279 = ORIENTED_EDGE ( 'NONE', *, *, #1779, .F. ) ;
#18280 = VERTEX_POINT ( 'NONE', #27602 ) ;
#18281 = APPLICATION_CONTEXT ( 'automotive_design' ) ;
#18282 = CARTESIAN_POINT ( 'NONE',  ( 109.9999999986357153, 137.0808454110858463, 100.0000000001515872 ) ) ;
#18283 = CARTESIAN_POINT ( 'NONE',  ( 79.99999999999991473, 140.0000000000000000, 100.0000000000000142 ) ) ;
#18284 = EDGE_CURVE ( 'NONE', #15498, #24050, #25460, .T. ) ;
#18285 = EDGE_LOOP ( 'NONE', ( #7360, #24614, #26620, #25441 ) ) ;
#18286 = ORIENTED_EDGE ( 'NONE', *, *, #3117, .T. ) ;
#18287 = CYLINDRICAL_SURFACE ( 'NONE', #26935, 5.000000000000004441 ) ;
#18288 = ADVANCED_FACE ( 'NONE', ( #23593 ), #3902, .F. ) ;
#18289 = DIRECTION ( 'NONE',  ( -0.8916010070300181001, 0.4528218681369723386, 0.000000000000000000 ) ) ;
#18290 = AXIS2_PLACEMENT_3D ( 'NONE', #1715, #8904, #28137 ) ;
#18291 = LINE ( 'NONE', #10090, #21510 ) ;
#18292 = ORIENTED_EDGE ( 'NONE', *, *, #2369, .F. ) ;
#18293 = CARTESIAN_POINT ( 'NONE',  ( 157.4999999999998579, 191.1594374136689964, 45.00000000000000000 ) ) ;
#18294 = ORIENTED_EDGE ( 'NONE', *, *, #10198, .F. ) ;
#18295 = DIRECTION ( 'NONE',  ( 0.000000000000000000, 0.000000000000000000, 1.000000000000000000 ) ) ;
#18296 = VECTOR ( 'NONE', #7138, 1000.000000000000000 ) ;
#18297 = AXIS2_PLACEMENT_3D ( 'NONE', #23027, #22612, #12128 ) ;
#18298 = LINE ( 'NONE', #27048, #16781 ) ;
#18299 = CARTESIAN_POINT ( 'NONE',  ( 157.4999999999998579, 80.81293708335913095, -45.00000000000000000 ) ) ;
#18300 = CARTESIAN_POINT ( 'NONE',  ( -27.05717226057298319, 127.9652800447362893, -17.51969307522723796 ) ) ;
#18301 = DIRECTION ( 'NONE',  ( -1.000000000000000000, 0.000000000000000000, 0.000000000000000000 ) ) ;
#18302 = ADVANCED_FACE ( 'NONE', ( #19280 ), #28022, .F. ) ;
#18303 = DIRECTION ( 'NONE',  ( 0.000000000000000000, 0.000000000000000000, 1.000000000000000000 ) ) ;
#18304 = DIRECTION ( 'NONE',  ( 0.000000000000000000, 0.000000000000000000, 1.000000000000000000 ) ) ;
#18305 = ORIENTED_EDGE ( 'NONE', *, *, #24535, .T. ) ;
#18306 = DIRECTION ( 'NONE',  ( -0.8916010070293283185, -0.4528218681383305855, 0.000000000000000000 ) ) ;
#18307 = CARTESIAN_POINT ( 'NONE',  ( -216.4421519707229606, 141.6000904446840991, 15.00000000000000000 ) ) ;
#18308 = CARTESIAN_POINT ( 'NONE',  ( 158.0000000000007674, 131.2243747372535267, 45.00000000000000000 ) ) ;
#18309 = CARTESIAN_POINT ( 'NONE',  ( 158.0000000000014211, 73.03537455708450921, -45.00000000000000000 ) ) ;
#18310 = ORIENTED_EDGE ( 'NONE', *, *, #13982, .F. ) ;
#18311 = CARTESIAN_POINT ( 'NONE',  ( -160.0000000000000284, 139.9999999999999716, -45.00000000000000000 ) ) ;
#18312 = ORIENTED_EDGE ( 'NONE', *, *, #24814, .T. ) ;
#18313 = EDGE_CURVE ( 'NONE', #23832, #12148, #14278, .T. ) ;
#18314 = VECTOR ( 'NONE', #16991, 1000.000000000000000 ) ;
#18315 = DIRECTION ( 'NONE',  ( -0.000000000000000000, -0.000000000000000000, -1.000000000000000000 ) ) ;
#18316 = DIRECTION ( 'NONE',  ( 0.9784193629480814058, 0.2066290158914539099, 0.000000000000000000 ) ) ;
#18317 = CARTESIAN_POINT ( 'NONE',  ( 39.99999999999996447, 59.99999999999981526, 80.00000000000001421 ) ) ;
#18318 = ORIENTED_EDGE ( 'NONE', *, *, #11095, .F. ) ;
#18319 = DIRECTION ( 'NONE',  ( 0.8916010070299781320, 0.4528218681370510534, 0.000000000000000000 ) ) ;
#18320 =( NAMED_UNIT ( * ) SI_UNIT ( $, .STERADIAN. ) SOLID_ANGLE_UNIT ( ) );
#18321 = VERTEX_POINT ( 'NONE', #3337 ) ;
#18322 = CIRCLE ( 'NONE', #17832, 1.000000000000000888 ) ;
#18323 = CARTESIAN_POINT ( 'NONE',  ( 158.0000000000005969, 148.7794997898028271, -45.00000000000000000 ) ) ;
#18324 = CARTESIAN_POINT ( 'NONE',  ( 94.61301761981503944, 240.5205114998973670, 8.728159109110571023 ) ) ;
#18325 = VERTEX_POINT ( 'NONE', #12129 ) ;
#18326 = AXIS2_PLACEMENT_3D ( 'NONE', #1920, #6380, #6522 ) ;
#18327 = ORIENTED_EDGE ( 'NONE', *, *, #3865, .F. ) ;
#18328 = CIRCLE ( 'NONE', #16482, 30.00000000000000000 ) ;
#18329 = DIRECTION ( 'NONE',  ( 0.000000000000000000, 0.000000000000000000, 1.000000000000000000 ) ) ;
#18330 = VERTEX_POINT ( 'NONE', #1191 ) ;
#18331 = EDGE_CURVE ( 'NONE', #22237, #8556, #3761, .T. ) ;
#18332 = ORIENTED_EDGE ( 'NONE', *, *, #10817, .F. ) ;
#18333 = EDGE_LOOP ( 'NONE', ( #25652, #9213, #6831, #15325 ) ) ;
#18334 = CARTESIAN_POINT ( 'NONE',  ( 109.9999999999999005, 259.4346755191849070, 44.02082925133874625 ) ) ;
#18335 = VECTOR ( 'NONE', #9377, 999.9999999999998863 ) ;
#18336 = DIRECTION ( 'NONE',  ( 0.000000000000000000, -1.000000000000000000, 0.000000000000000000 ) ) ;
#18337 = AXIS2_PLACEMENT_3D ( 'NONE', #3048, #13855, #20441 ) ;
#18338 = LINE ( 'NONE', #7565, #15153 ) ;
#18339 = EDGE_CURVE ( 'NONE', #13911, #10408, #11535, .T. ) ;
#18340 = CARTESIAN_POINT ( 'NONE',  ( 107.3061218092339715, 127.3934823308176760, -87.81249999970602005 ) ) ;
#18341 = AXIS2_PLACEMENT_3D ( 'NONE', #290, #6737, #8760 ) ;
#18342 = PLANE ( 'NONE',  #12653 ) ;
#18343 = DIRECTION ( 'NONE',  ( 1.000000000000000000, 0.000000000000000000, -0.000000000000000000 ) ) ;
#18344 = DIRECTION ( 'NONE',  ( -0.000000000000000000, -0.000000000000000000, -1.000000000000000000 ) ) ;
#18345 = DIRECTION ( 'NONE',  ( 1.000000000000000000, 0.000000000000000000, 0.000000000000000000 ) ) ;
#18346 = LINE ( 'NONE', #7572, #19793 ) ;
#18347 = LINE ( 'NONE', #15774, #18296 ) ;
#18348 = DIRECTION ( 'NONE',  ( 1.000000000000000000, 0.000000000000000000, 0.000000000000000000 ) ) ;
#18349 = ORIENTED_EDGE ( 'NONE', *, *, #18828, .T. ) ;
#18351 = EDGE_CURVE ( 'NONE', #27657, #26801, #13829, .T. ) ;
#18350 = AXIS2_PLACEMENT_3D ( 'NONE', #21957, #24544, #6872 ) ;
#18352 = DIRECTION ( 'NONE',  ( -0.000000000000000000, -0.000000000000000000, -1.000000000000000000 ) ) ;
#18353 = DIRECTION ( 'NONE',  ( 0.4528218681382463751, 0.8916010070293711731, -0.000000000000000000 ) ) ;
#18354 = EDGE_CURVE ( 'NONE', #13425, #8035, #15947, .T. ) ;
#18355 = CARTESIAN_POINT ( 'NONE',  ( 158.0000000000000853, 200.9369999399436892, 45.00000000000000000 ) ) ;
#18356 = ORIENTED_EDGE ( 'NONE', *, *, #18726, .T. ) ;
#18357 = AXIS2_PLACEMENT_3D ( 'NONE', #11820, #27026, #20134 ) ;
#18358 = LINE ( 'NONE', #24959, #601 ) ;
#18359 = ORIENTED_EDGE ( 'NONE', *, *, #9598, .T. ) ;
#18360 = ORIENTED_EDGE ( 'NONE', *, *, #25671, .T. ) ;
#18361 = VECTOR ( 'NONE', #5547, 1000.000000000000000 ) ;
#18362 = ORIENTED_EDGE ( 'NONE', *, *, #2367, .F. ) ;
#18363 = ORIENTED_EDGE ( 'NONE', *, *, #11513, .T. ) ;
#18364 = VERTEX_POINT ( 'NONE', #12975 ) ;
#18365 = CARTESIAN_POINT ( 'NONE',  ( -97.95444496743660068, 136.1562174567784496, 13.53396451897430985 ) ) ;
#18366 = DIRECTION ( 'NONE',  ( 0.000000000000000000, 1.000000000000000000, 0.000000000000000000 ) ) ;
#18367 = DIRECTION ( 'NONE',  ( 1.000000000000000000, -0.000000000000000000, -0.000000000000000000 ) ) ;
#18368 = UNCERTAINTY_MEASURE_WITH_UNIT (LENGTH_MEASURE( 1.000000000000000082E-05 ), #8943, 'distance_accuracy_value', 'NONE');
#18369 = CARTESIAN_POINT ( 'NONE',  ( -24.75792395070879337, 129.2472835422605897, 15.64968610871202515 ) ) ;
#18370 = CARTESIAN_POINT ( 'NONE',  ( -213.7829002709373754, 55.69945581370511434, 42.78690303009008034 ) ) ;
#18371 = LINE ( 'NONE', #18090, #11618 ) ;
#18372 = CARTESIAN_POINT ( 'NONE',  ( -101.6645475182762226, 135.8110788931456057, -13.60253974807226029 ) ) ;
#18373 = AXIS2_PLACEMENT_3D ( 'NONE', #4961, #26948, #18199 ) ;
#18374 = DIRECTION ( 'NONE',  ( -0.000000000000000000, 1.000000000000000000, -0.000000000000000000 ) ) ;
#18375 = DIRECTION ( 'NONE',  ( -0.4528218681382848443, -0.8916010070293515222, 0.000000000000000000 ) ) ;
#18376 = ADVANCED_FACE ( 'NONE', ( #11349 ), #17944, .F. ) ;
#18377 = LINE ( 'NONE', #25257, #2329 ) ;
#18378 = DIRECTION ( 'NONE',  ( 4.540956701092242152E-16, 1.000000000000000000, 0.000000000000000000 ) ) ;
#18379 = CARTESIAN_POINT ( 'NONE',  ( 94.38583646782731762, 113.6320904521816857, 75.15625000028097702 ) ) ;
#18380 = ADVANCED_FACE ( 'NONE', ( #26695 ), #19566, .F. ) ;
#18381 = VECTOR ( 'NONE', #27893, 1000.000000000000000 ) ;
#18382 = CARTESIAN_POINT ( 'NONE',  ( 69.99612328191057031, 261.2290884209365345, 45.00000000000000000 ) ) ;
#18383 = DIRECTION ( 'NONE',  ( -0.000000000000000000, -0.000000000000000000, -1.000000000000000000 ) ) ;
#18385 = ORIENTED_EDGE ( 'NONE', *, *, #19238, .T. ) ;
#18384 = ORIENTED_EDGE ( 'NONE', *, *, #13776, .F. ) ;
#18386 = LINE ( 'NONE', #9052, #19711 ) ;
#18387 = FACE_OUTER_BOUND ( 'NONE', #2766, .T. ) ;
#18388 = VERTEX_POINT ( 'NONE', #6487 ) ;
#18389 = VERTEX_POINT ( 'NONE', #7175 ) ;
#18390 = FACE_OUTER_BOUND ( 'NONE', #2463, .T. ) ;
#18391 = CIRCLE ( 'NONE', #11517, 30.00000000000000000 ) ;
#18392 = CARTESIAN_POINT ( 'NONE',  ( -86.54521714544338806, 134.8061557207362000, 15.45301935095626611 ) ) ;
#18393 = EDGE_CURVE ( 'NONE', #18911, #24637, #6204, .T. ) ;
#18394 = ORIENTED_EDGE ( 'NONE', *, *, #7241, .T. ) ;
#18395 = ORIENTED_EDGE ( 'NONE', *, *, #24657, .T. ) ;
#18396 = CARTESIAN_POINT ( 'NONE',  ( 144.9999999999998863, 220.0000000000000284, 99.00000000000001421 ) ) ;
#18397 = LINE ( 'NONE', #7485, #18679 ) ;
#18398 = VECTOR ( 'NONE', #2134, 1000.000000000000000 ) ;
#18399 = EDGE_CURVE ( 'NONE', #12077, #4176, #8510, .T. ) ;
#18400 = DIRECTION ( 'NONE',  ( -0.000000000000000000, -0.000000000000000000, -1.000000000000000000 ) ) ;
#18401 = CARTESIAN_POINT ( 'NONE',  ( 92.91656858538189567, 230.8754161317235400, -17.91819948002591190 ) ) ;
#18402 = DIRECTION ( 'NONE',  ( 0.000000000000000000, 1.000000000000000000, 0.000000000000000000 ) ) ;
#18403 = EDGE_CURVE ( 'NONE', #23120, #8173, #28168, .T. ) ;
#18404 = CARTESIAN_POINT ( 'NONE',  ( 267.4999999999996021, 194.4107529906318064, -100.0000000000000000 ) ) ;
#18405 = CARTESIAN_POINT ( 'NONE',  ( -209.5875676835875083, 74.18578632021306873, -35.35260769160358052 ) ) ;
#18406 = EDGE_CURVE ( 'NONE', #1600, #21920, #8299, .T. ) ;
#18407 = CARTESIAN_POINT ( 'NONE',  ( 157.9999999999997442, 254.1102501050980322, 45.00000000000000000 ) ) ;
#18408 = EDGE_CURVE ( 'NONE', #7534, #1460, #26019, .T. ) ;
#18409 = PLANE ( 'NONE',  #22537 ) ;
#18410 = DIRECTION ( 'NONE',  ( -0.8916010070296124246, -0.4528218681377710886, 0.000000000000000000 ) ) ;
#18411 = DIRECTION ( 'NONE',  ( 1.000000000000000000, 0.000000000000000000, 0.000000000000000000 ) ) ;
#18412 = ORIENTED_EDGE ( 'NONE', *, *, #17487, .T. ) ;
#18413 = CARTESIAN_POINT ( 'NONE',  ( 110.9201389036588949, 220.0000000000000284, -84.99999999999997158 ) ) ;
#18414 = AXIS2_PLACEMENT_3D ( 'NONE', #2716, #4440, #15524 ) ;
#18415 = CARTESIAN_POINT ( 'NONE',  ( -234.1955688336202854, 78.70261838805045329, 15.19002172608710843 ) ) ;
#18416 = LINE ( 'NONE', #27030, #18148 ) ;
#18417 = ORIENTED_EDGE ( 'NONE', *, *, #7486, .T. ) ;
#18418 = DIRECTION ( 'NONE',  ( 1.000000000000000000, 0.000000000000000000, 0.000000000000000000 ) ) ;
#18419 = ORIENTED_EDGE ( 'NONE', *, *, #1975, .T. ) ;
#18420 = CARTESIAN_POINT ( 'NONE',  ( 85.90765579575223398, 110.5723347142863702, 70.58593750014345858 ) ) ;
#18421 = DIRECTION ( 'NONE',  ( 0.000000000000000000, 0.000000000000000000, -1.000000000000000000 ) ) ;
#18422 = ORIENTED_EDGE ( 'NONE', *, *, #21976, .F. ) ;
#18423 = ORIENTED_EDGE ( 'NONE', *, *, #13077, .F. ) ;
#18424 = DIRECTION ( 'NONE',  ( 0.000000000000000000, 0.000000000000000000, 1.000000000000000000 ) ) ;
#18425 = AXIS2_PLACEMENT_3D ( 'NONE', #26955, #16199, #25085 ) ;
#18426 = LINE ( 'NONE', #5206, #1478 ) ;
#18427 = DIRECTION ( 'NONE',  ( -0.000000000000000000, -0.000000000000000000, -1.000000000000000000 ) ) ;
#18428 = VERTEX_POINT ( 'NONE', #26849 ) ;
#18429 = PLANE ( 'NONE',  #21523 ) ;
#18430 = ORIENTED_EDGE ( 'NONE', *, *, #20641, .T. ) ;
#18431 = CIRCLE ( 'NONE', #18026, 5.999999999999991118 ) ;
#18432 = AXIS2_PLACEMENT_3D ( 'NONE', #16725, #19015, #3777 ) ;
#18433 = CARTESIAN_POINT ( 'NONE',  ( 158.0000000000012790, 85.57474959461971764, -45.00000000000000000 ) ) ;
#18434 = EDGE_CURVE ( 'NONE', #27491, #583, #24697, .T. ) ;
#18435 = CIRCLE ( 'NONE', #6038, 66.76834224489934400 ) ;
#18436 = EDGE_CURVE ( 'NONE', #17770, #18330, #9186, .T. ) ;
#18437 = CARTESIAN_POINT ( 'NONE',  ( -156.2917263574996127, 178.8555734514394828, -13.00000000000000000 ) ) ;
#18438 = FACE_OUTER_BOUND ( 'NONE', #27271, .T. ) ;
#18439 = CARTESIAN_POINT ( 'NONE',  ( -0.3773123655229073670, 134.1569627555659849, -15.55970061581417241 ) ) ;
#18440 = PLANE ( 'NONE',  #27905 ) ;
#18441 = LINE ( 'NONE', #9822, #10129 ) ;
#18442 = CARTESIAN_POINT ( 'NONE',  ( 162.4217010148293525, 207.8312982882352173, -139.9035143180224736 ) ) ;
#18443 = ORIENTED_EDGE ( 'NONE', *, *, #20641, .F. ) ;
#18444 = FACE_OUTER_BOUND ( 'NONE', #24436, .T. ) ;
#18445 = EDGE_CURVE ( 'NONE', #23757, #26144, #7405, .T. ) ;
#18446 = LINE ( 'NONE', #14146, #13407 ) ;
#18447 = DIRECTION ( 'NONE',  ( -0.8916010070293409751, -0.4528218681383056610, 0.000000000000000000 ) ) ;
#18448 = ORIENTED_EDGE ( 'NONE', *, *, #21024, .T. ) ;
#18449 = DIRECTION ( 'NONE',  ( -0.8916010070293483025, -0.4528218681382912281, 0.000000000000000000 ) ) ;
#18450 = VERTEX_POINT ( 'NONE', #9333 ) ;
#18451 = PRODUCT_DEFINITION ( 'UNKNOWN', '', #1929, #274 ) ;
#18452 = VECTOR ( 'NONE', #13156, 1000.000000000000000 ) ;
#18453 = DIRECTION ( 'NONE',  ( 1.000000000000000000, 0.000000000000000000, 0.000000000000000000 ) ) ;
#18454 = LINE ( 'NONE', #9969, #18814 ) ;
#18455 = CARTESIAN_POINT ( 'NONE',  ( 217.4999999999996305, 258.6181251126050711, 6.000000000000019540 ) ) ;
#18456 = VERTEX_POINT ( 'NONE', #19422 ) ;
#18457 = DIRECTION ( 'NONE',  ( -0.000000000000000000, 0.000000000000000000, -1.000000000000000000 ) ) ;
#18458 = LINE ( 'NONE', #12147, #23950 ) ;
#18459 = CIRCLE ( 'NONE', #22576, 5.999999999999991118 ) ;
#18460 = ORIENTED_EDGE ( 'NONE', *, *, #12650, .T. ) ;
#18461 = DIRECTION ( 'NONE',  ( 0.000000000000000000, 1.214306433183764966E-16, -1.000000000000000000 ) ) ;
#18462 = CARTESIAN_POINT ( 'NONE',  ( 101.0658546243658407, 243.3257901681003261, 15.10247091754472493 ) ) ;
#18463 = ORIENTED_EDGE ( 'NONE', *, *, #16587, .F. ) ;
#18464 = EDGE_LOOP ( 'NONE', ( #195, #12694, #17517, #16794 ) ) ;
#18465 = LINE ( 'NONE', #5100, #17283 ) ;
#18466 = ORIENTED_EDGE ( 'NONE', *, *, #19, .F. ) ;
#18467 = ORIENTED_EDGE ( 'NONE', *, *, #1210, .F. ) ;
#18468 = ORIENTED_EDGE ( 'NONE', *, *, #15362, .F. ) ;
#18469 = AXIS2_PLACEMENT_3D ( 'NONE', #942, #22648, #2953 ) ;
#18470 = CARTESIAN_POINT ( 'NONE',  ( 158.0000000000009663, 113.6692496847042264, 45.00000000000000000 ) ) ;
#18471 = EDGE_CURVE ( 'NONE', #14063, #7534, #5005, .T. ) ;
#18472 = EDGE_CURVE ( 'NONE', #26566, #3490, #4863, .T. ) ;
#18473 = VECTOR ( 'NONE', #9929, 1000.000000000000114 ) ;
#18474 = CARTESIAN_POINT ( 'NONE',  ( -56.48697296830715686, 1.968917815184006985E-15, 100.0000000000000000 ) ) ;
#18475 = FACE_OUTER_BOUND ( 'NONE', #10693, .T. ) ;
#18476 = AXIS2_PLACEMENT_3D ( 'NONE', #22415, #4882, #24996 ) ;
#18477 = AXIS2_PLACEMENT_3D ( 'NONE', #3635, #12844, #16863 ) ;
#18478 = DIRECTION ( 'NONE',  ( -0.8916010070296327417, -0.4528218681377311761, 0.000000000000000000 ) ) ;
#18479 = CARTESIAN_POINT ( 'NONE',  ( 65.00000000000000000, -120.0000000000000711, 76.02500000000001990 ) ) ;
#18480 = FACE_OUTER_BOUND ( 'NONE', #6634, .T. ) ;
#18481 = LINE ( 'NONE', #22930, #14515 ) ;
#18482 = DIRECTION ( 'NONE',  ( -0.000000000000000000, 1.000000000000000000, -1.387778780781445429E-16 ) ) ;
#18483 = CARTESIAN_POINT ( 'NONE',  ( 93.17300876009500143, -24.96563245364655259, 45.00000000000000000 ) ) ;
#18484 = LINE ( 'NONE', #20914, #1973 ) ;
#18485 = ORIENTED_EDGE ( 'NONE', *, *, #24404, .F. ) ;
#18486 = ADVANCED_FACE ( 'NONE', ( #11497 ), #15124, .F. ) ;
#18487 = ADVANCED_FACE ( 'NONE', ( #18236 ), #21721, .F. ) ;
#18488 = DIRECTION ( 'NONE',  ( -0.8916010070293483025, -0.4528218681382912281, 0.000000000000000000 ) ) ;
#18489 = CARTESIAN_POINT ( 'NONE',  ( 157.4999999999998579, 100.8759371434154701, 45.00000000000000000 ) ) ;
#18490 = LINE ( 'NONE', #7294, #79 ) ;
#18491 = EDGE_LOOP ( 'NONE', ( #4593, #3430, #23478, #11598 ) ) ;
#18492 = VECTOR ( 'NONE', #7972, 1000.000000000000227 ) ;
#18493 = CIRCLE ( 'NONE', #12984, 5.000000000000004441 ) ;
#18494 = CYLINDRICAL_SURFACE ( 'NONE', #14378, 10.00000000000000888 ) ;
#18495 = VERTEX_POINT ( 'NONE', #11645 ) ;
#18496 = DIRECTION ( 'NONE',  ( 0.8916010070293995948, 0.4528218681381900312, 0.000000000000000000 ) ) ;
#18497 = VECTOR ( 'NONE', #9044, 1000.000000000000000 ) ;
#18498 = EDGE_CURVE ( 'NONE', #9774, #23905, #20383, .T. ) ;
#18499 = ORIENTED_EDGE ( 'NONE', *, *, #2297, .T. ) ;
#18500 = AXIS2_PLACEMENT_3D ( 'NONE', #9562, #7551, #20471 ) ;
#18501 = EDGE_CURVE ( 'NONE', #14199, #12605, #3414, .T. ) ;
#18502 = MANIFOLD_SOLID_BREP ( 'Slot', #21427 ) ;
#18503 = EDGE_LOOP ( 'NONE', ( #8573, #8345, #26286, #18219 ) ) ;
#18504 = ORIENTED_EDGE ( 'NONE', *, *, #17717, .T. ) ;
#18505 = VERTEX_POINT ( 'NONE', #7601 ) ;
#18506 = CARTESIAN_POINT ( 'NONE',  ( -52.43880247855167909, 133.2613159911169021, 14.19473240045777374 ) ) ;
#18507 = CARTESIAN_POINT ( 'NONE',  ( 158.0000000000000853, 196.4291249324366504, -45.00000000000000000 ) ) ;
#18508 = CARTESIAN_POINT ( 'NONE',  ( -37.82257053376181233, 71.03850157808263077, 99.00000000000000000 ) ) ;
#18509 = CARTESIAN_POINT ( 'NONE',  ( -42.53273978471832351, 130.9733465240572343, -14.93735646117641558 ) ) ;
#18510 = CARTESIAN_POINT ( 'NONE',  ( -28.13809330698875755, 129.1551964303678801, 15.69125710151050868 ) ) ;
#18511 = VECTOR ( 'NONE', #10768, 1000.000000000000000 ) ;
#18512 = DIRECTION ( 'NONE',  ( 0.000000000000000000, 0.000000000000000000, 1.000000000000000000 ) ) ;
#18513 = CARTESIAN_POINT ( 'NONE',  ( 2.114710523095537590E-14, -160.0000000000001137, 110.0000000000000284 ) ) ;
#18514 = LINE ( 'NONE', #22687, #12223 ) ;
#18515 = VECTOR ( 'NONE', #4649, 1000.000000000000000 ) ;
#18516 = CARTESIAN_POINT ( 'NONE',  ( -17.24491960465746132, 75.97823757117562593, 95.00000000000000000 ) ) ;
#18517 = DIRECTION ( 'NONE',  ( 0.000000000000000000, 0.000000000000000000, 1.000000000000000000 ) ) ;
#18518 = VECTOR ( 'NONE', #19776, 1000.000000000000000 ) ;
#18519 = FACE_OUTER_BOUND ( 'NONE', #12191, .T. ) ;
#18520 = FACE_OUTER_BOUND ( 'NONE', #11904, .T. ) ;
#18521 = CARTESIAN_POINT ( 'NONE',  ( 164.9999999999998579, 220.0000000000000284, -122.9999999999999574 ) ) ;
#18522 = ADVANCED_FACE ( 'NONE', ( #7738 ), #974, .T. ) ;
#18523 = DIRECTION ( 'NONE',  ( -0.000000000000000000, 1.000000000000000000, -1.387778780781445429E-16 ) ) ;
#18524 = CARTESIAN_POINT ( 'NONE',  ( 118.9718481642231609, 125.5986290015685398, -100.0000000000000142 ) ) ;
#18525 = FACE_OUTER_BOUND ( 'NONE', #16652, .T. ) ;
#18527 = ORIENTED_EDGE ( 'NONE', *, *, #11660, .T. ) ;
#18526 = EDGE_LOOP ( 'NONE', ( #22381, #4062, #19583, #5469 ) ) ;
#18528 = CARTESIAN_POINT ( 'NONE',  ( -12.24491960465745599, 24.64876300893806160, 95.00000000000000000 ) ) ;
#18529 = ORIENTED_EDGE ( 'NONE', *, *, #28285, .T. ) ;
#18530 = VECTOR ( 'NONE', #12655, 1000.000000000000000 ) ;
#18531 = ORIENTED_EDGE ( 'NONE', *, *, #1946, .T. ) ;
#18532 = EDGE_LOOP ( 'NONE', ( #14472, #22784, #11766, #7196 ) ) ;
#18533 = CIRCLE ( 'NONE', #18976, 19.68410787789781580 ) ;
#18534 = VERTEX_POINT ( 'NONE', #11786 ) ;
#18535 = CARTESIAN_POINT ( 'NONE',  ( 111.9999999999968878, -1.554312234475174324E-12, 45.00000000000000000 ) ) ;
#18536 = EDGE_CURVE ( 'NONE', #12559, #6913, #18377, .T. ) ;
#18537 = DIRECTION ( 'NONE',  ( 1.000000000000000000, 0.000000000000000000, -0.000000000000000000 ) ) ;
#18538 = ADVANCED_FACE ( 'NONE', ( #14350 ), #23109, .T. ) ;
#18539 = CARTESIAN_POINT ( 'NONE',  ( 232.4999999999996305, 83.06687458711267880, -36.86484227207694175 ) ) ;
#18540 = EDGE_CURVE ( 'NONE', #17607, #27590, #21084, .T. ) ;
#18541 = LINE ( 'NONE', #18122, #27235 ) ;
#18542 = CARTESIAN_POINT ( 'NONE',  ( 109.9999999999999005, 3.816391647148972452E-14, 25.00000000000000000 ) ) ;
#18543 = DIRECTION ( 'NONE',  ( 0.000000000000000000, 0.000000000000000000, -1.000000000000000000 ) ) ;
#18544 = CARTESIAN_POINT ( 'NONE',  ( 157.9999999999996874, 266.1417501351260171, -45.00000000000000000 ) ) ;
#18545 = CARTESIAN_POINT ( 'NONE',  ( -211.5579651433048411, 73.08537964810861354, -31.40200346762902939 ) ) ;
#18546 = VECTOR ( 'NONE', #7455, 1000.000000000000114 ) ;
#18547 = CARTESIAN_POINT ( 'NONE',  ( 110.7507446791215102, 202.3364611620586402, -139.9035143180225020 ) ) ;
#18548 = DIRECTION ( 'NONE',  ( 1.000000000000000000, 0.000000000000000000, 0.000000000000000000 ) ) ;
#18549 = DIRECTION ( 'NONE',  ( -0.3897722486529259234, 0.9209112846414913012, 1.118268497331688440E-16 ) ) ;
#18550 = AXIS2_PLACEMENT_3D ( 'NONE', #17837, #11539, #6919 ) ;
#18551 = FACE_OUTER_BOUND ( 'NONE', #19757, .T. ) ;
#18552 = ORIENTED_EDGE ( 'NONE', *, *, #9628, .T. ) ;
#18553 = CARTESIAN_POINT ( 'NONE',  ( 157.4999999999996589, 278.9350626764145318, -45.00000000000000000 ) ) ;
#18554 = CARTESIAN_POINT ( 'NONE',  ( -227.4113622183683106, 63.29489605847815881, 7.985794955240776538 ) ) ;
#18555 = DIRECTION ( 'NONE',  ( 1.000000000000000000, 0.000000000000000000, -0.000000000000000000 ) ) ;
#18556 = ORIENTED_EDGE ( 'NONE', *, *, #5477, .F. ) ;
#18557 =( NAMED_UNIT ( * ) SI_UNIT ( $, .STERADIAN. ) SOLID_ANGLE_UNIT ( ) );
#18558 = VERTEX_POINT ( 'NONE', #23248 ) ;
#18559 = DIRECTION ( 'NONE',  ( 0.8018642810807392607, 0.5975062131282562472, 5.456026535785215050E-16 ) ) ;
#18560 = CARTESIAN_POINT ( 'NONE',  ( 79.99999999999990052, 240.0000000000000284, -5.000000000000004441 ) ) ;
#18561 = ORIENTED_EDGE ( 'NONE', *, *, #11115, .T. ) ;
#18562 = EDGE_CURVE ( 'NONE', #4740, #21445, #27129, .T. ) ;
#18563 = VECTOR ( 'NONE', #21718, 1000.000000000000000 ) ;
#18564 = ORIENTED_EDGE ( 'NONE', *, *, #25247, .F. ) ;
#18565 = EDGE_CURVE ( 'NONE', #2405, #12219, #1405, .T. ) ;
#18566 = ADVANCED_FACE ( 'NONE', ( #26986 ), #18791, .F. ) ;
#18567 = CARTESIAN_POINT ( 'NONE',  ( 158.0000000000009379, 116.1771246922112653, 45.00000000000000000 ) ) ;
#18568 = EDGE_CURVE ( 'NONE', #9863, #13271, #24345, .T. ) ;
#18569 = FACE_OUTER_BOUND ( 'NONE', #15461, .T. ) ;
#18570 = ORIENTED_EDGE ( 'NONE', *, *, #25529, .F. ) ;
#18571 = DIRECTION ( 'NONE',  ( -1.321694076934710155E-16, 1.000000000000000000, 0.000000000000000000 ) ) ;
#18572 = VERTEX_POINT ( 'NONE', #22690 ) ;
#18573 = VECTOR ( 'NONE', #17768, 1000.000000000000000 ) ;
#18574 = CARTESIAN_POINT ( 'NONE',  ( -248.1546605714623013, -91.18033988749901653, -16.91094714394370158 ) ) ;
#18575 = LINE ( 'NONE', #25455, #22732 ) ;
#18576 = DIRECTION ( 'NONE',  ( 0.000000000000000000, 0.000000000000000000, 1.000000000000000000 ) ) ;
#18577 = CARTESIAN_POINT ( 'NONE',  ( 134.9999999999998579, 220.0000000000000284, 45.00000000000000000 ) ) ;
#18578 = CARTESIAN_POINT ( 'NONE',  ( 157.9999999999996305, 286.2047501951820436, 45.00000000000000000 ) ) ;
#18579 = CARTESIAN_POINT ( 'NONE',  ( 158.0000000000008811, 121.1928747072253572, 45.00000000000000000 ) ) ;
#18580 = DIRECTION ( 'NONE',  ( 1.000000000000000000, 2.602085213965211135E-16, -0.000000000000000000 ) ) ;
#18581 = ORIENTED_EDGE ( 'NONE', *, *, #6350, .F. ) ;
#18582 = CARTESIAN_POINT ( 'NONE',  ( 158.0000000000004832, 161.3188748273380213, -45.00000000000000000 ) ) ;
#18583 = DIRECTION ( 'NONE',  ( 0.000000000000000000, 0.000000000000000000, 1.000000000000000000 ) ) ;
#18584 = CARTESIAN_POINT ( 'NONE',  ( 367.4999999999996021, -5.589247009368136787, -100.0000000000000142 ) ) ;
#18585 = EDGE_LOOP ( 'NONE', ( #13068, #18805, #22918, #2656 ) ) ;
#18586 = VECTOR ( 'NONE', #16809, 1000.000000000000000 ) ;
#18587 = CARTESIAN_POINT ( 'NONE',  ( 73.69623568533953062, -15.56365422765611051, 45.00000000000000000 ) ) ;
#18588 = VERTEX_POINT ( 'NONE', #7461 ) ;
#18589 = CARTESIAN_POINT ( 'NONE',  ( 410.1240808061609187, 61.15703788601284430, -145.0000000000000000 ) ) ;
#18590 = CARTESIAN_POINT ( 'NONE',  ( 117.5127944162877753, 203.5381304684075019, 45.00000000000000000 ) ) ;
#18591 = ORIENTED_EDGE ( 'NONE', *, *, #1400, .F. ) ;
#18592 = CARTESIAN_POINT ( 'NONE',  ( 158.0000000000008811, 123.1928747072253572, -45.00000000000000000 ) ) ;
#18593 = VECTOR ( 'NONE', #17881, 1000.000000000000114 ) ;
#18594 = ORIENTED_EDGE ( 'NONE', *, *, #5323, .F. ) ;
#18595 = EDGE_CURVE ( 'NONE', #21378, #21916, #1264, .T. ) ;
#18596 = ADVANCED_FACE ( 'NONE', ( #18519 ), #22829, .F. ) ;
#18597 = CARTESIAN_POINT ( 'NONE',  ( -122.3725384480337226, 131.4093997917716763, 16.24372036387202201 ) ) ;
#18598 = EDGE_LOOP ( 'NONE', ( #16022, #6440, #5871, #20291, #26188, #14367, #13154, #10418, #6972, #21066, #10726, #10973, #9775, #26020, #14446 ) ) ;
#18599 = ORIENTED_EDGE ( 'NONE', *, *, #21294, .F. ) ;
#18600 = ADVANCED_FACE ( 'NONE', ( #19354 ), #12907, .F. ) ;
#18601 = CARTESIAN_POINT ( 'NONE',  ( 158.0000000000006821, 140.7479997597746433, 45.00000000000000000 ) ) ;
#18602 = ORIENTED_EDGE ( 'NONE', *, *, #14999, .T. ) ;
#18603 = EDGE_CURVE ( 'NONE', #25748, #3224, #2351, .T. ) ;
#18604 = VECTOR ( 'NONE', #10697, 999.9999999999998863 ) ;
#18605 = ORIENTED_EDGE ( 'NONE', *, *, #23272, .T. ) ;
#18606 = EDGE_LOOP ( 'NONE', ( #23713, #27177, #13517, #12220 ) ) ;
#18607 = CIRCLE ( 'NONE', #22277, 5.000000000000004441 ) ;
#18608 = CIRCLE ( 'NONE', #6665, 8.000000000000000000 ) ;
#18609 = DIRECTION ( 'NONE',  ( -0.8916010070293483025, -0.4528218681382912281, 0.000000000000000000 ) ) ;
#18610 = LINE ( 'NONE', #13607, #1148 ) ;
#18611 = DIRECTION ( 'NONE',  ( -0.000000000000000000, -0.000000000000000000, -1.000000000000000000 ) ) ;
#18612 = AXIS2_PLACEMENT_3D ( 'NONE', #11216, #17957, #17524 ) ;
#18613 = LINE ( 'NONE', #26811, #24813 ) ;
#18614 = CYLINDRICAL_SURFACE ( 'NONE', #10358, 5.999999999999977796 ) ;
#18615 = CARTESIAN_POINT ( 'NONE',  ( 158.0000000000001705, 188.9054999099155054, -45.00000000000000000 ) ) ;
#18616 = CARTESIAN_POINT ( 'NONE',  ( -160.0000000000000568, 118.4170923319166775, -21.37420696376537776 ) ) ;
#18617 = CARTESIAN_POINT ( 'NONE',  ( -160.0000000000000568, 90.00000000000001421, 80.00000000000001421 ) ) ;
#18618 = CARTESIAN_POINT ( 'NONE',  ( 134.9999999999998579, 220.0000000000000284, -169.9999999999999716 ) ) ;
#18619 = DIRECTION ( 'NONE',  ( 1.321694076934710155E-16, -1.000000000000000000, 0.000000000000000000 ) ) ;
#18620 = VERTEX_POINT ( 'NONE', #23527 ) ;
#18621 = CARTESIAN_POINT ( 'NONE',  ( 139.9869122110687840, 242.4751130497508314, 45.00000000000000000 ) ) ;
#18622 = CARTESIAN_POINT ( 'NONE',  ( 15.75831141662812840, 89.44692362408399333, 98.47400872637959424 ) ) ;
#18623 = VECTOR ( 'NONE', #15375, 1000.000000000000000 ) ;
#18624 =( NAMED_UNIT ( * ) SI_UNIT ( $, .STERADIAN. ) SOLID_ANGLE_UNIT ( ) );
#18625 = FACE_OUTER_BOUND ( 'NONE', #5444, .T. ) ;
#18626 = ADVANCED_FACE ( 'NONE', ( #21652 ), #3842, .F. ) ;
#18627 = EDGE_LOOP ( 'NONE', ( #11007, #17317, #14901, #16599 ) ) ;
#18628 = CIRCLE ( 'NONE', #13596, 10.71881775658151170 ) ;
#18629 = AXIS2_PLACEMENT_3D ( 'NONE', #20892, #16867, #21028 ) ;
#18630 = ADVANCED_FACE ( 'NONE', ( #3977 ), #529, .F. ) ;
#18631 = CARTESIAN_POINT ( 'NONE',  ( 157.4999999999998579, 198.6830624361901414, 45.00000000000000000 ) ) ;
#18632 = ORIENTED_EDGE ( 'NONE', *, *, #20375, .F. ) ;
#18633 = PLANE ( 'NONE',  #27776 ) ;
#18634 = VERTEX_POINT ( 'NONE', #10746 ) ;
#18635 = AXIS2_PLACEMENT_3D ( 'NONE', #25458, #9819, #23307 ) ;
#18636 = EDGE_LOOP ( 'NONE', ( #28169, #16000, #10114, #10869 ) ) ;
#18637 = ORIENTED_EDGE ( 'NONE', *, *, #10526, .F. ) ;
#18638 = ORIENTED_EDGE ( 'NONE', *, *, #22065, .T. ) ;
#18639 = EDGE_LOOP ( 'NONE', ( #2976, #16418, #9591, #14368 ) ) ;
#18640 = CARTESIAN_POINT ( 'NONE',  ( 193.7634559672933676, 193.7634559672857790, -45.00000000000000000 ) ) ;
#18641 = DIRECTION ( 'NONE',  ( 0.6681556583950049033, -0.7440215159219103480, 0.000000000000000000 ) ) ;
#18642 = CARTESIAN_POINT ( 'NONE',  ( -211.0641392867345871, -220.0000000000001137, -91.81659942089190451 ) ) ;
#18643 = ADVANCED_FACE ( 'NONE', ( #17201, #6145 ), #10315, .F. ) ;
#18644 = CARTESIAN_POINT ( 'NONE',  ( -90.20499964516722002, 136.4340600182870844, -13.48772813831959283 ) ) ;
#18645 = VECTOR ( 'NONE', #4168, 1000.000000000000000 ) ;
#18646 = CARTESIAN_POINT ( 'NONE',  ( -107.3221550338875687, 17.24192588826928585, 83.00000000000001421 ) ) ;
#18647 = CARTESIAN_POINT ( 'NONE',  ( -214.2335385402416534, 55.09354448559309958, 44.71599978583095236 ) ) ;
#18648 = LINE ( 'NONE', #27391, #10478 ) ;
#18649 = CARTESIAN_POINT ( 'NONE',  ( -160.0000000000000284, 109.9999999999999432, 45.00000000000000000 ) ) ;
#18650 = CARTESIAN_POINT ( 'NONE',  ( 79.99999999999997158, 95.03452022453005554, -96.03494797070611355 ) ) ;
#18651 = CARTESIAN_POINT ( 'NONE',  ( -217.7945318781847845, 87.80073750458967652, -17.67178672655967375 ) ) ;
#18652 = VECTOR ( 'NONE', #23211, 1000.000000000000114 ) ;
#18653 = DIRECTION ( 'NONE',  ( 0.000000000000000000, 0.000000000000000000, 1.000000000000000000 ) ) ;
#18654 = DIRECTION ( 'NONE',  ( -0.8916010070294605461, -0.4528218681380702382, 0.000000000000000000 ) ) ;
#18655 = VERTEX_POINT ( 'NONE', #16919 ) ;
#18656 = EDGE_CURVE ( 'NONE', #4479, #21343, #25816, .T. ) ;
#18657 = CARTESIAN_POINT ( 'NONE',  ( -39.33244318694370634, -19.07742562058452052, 99.88564812209577326 ) ) ;
#18658 = DIRECTION ( 'NONE',  ( 0.000000000000000000, 0.000000000000000000, 1.000000000000000000 ) ) ;
#18659 = CARTESIAN_POINT ( 'NONE',  ( 158.0000000000004547, 165.8267498348450886, -45.00000000000000000 ) ) ;
#18661 = ORIENTED_EDGE ( 'NONE', *, *, #18436, .F. ) ;
#18660 = ORIENTED_EDGE ( 'NONE', *, *, #14481, .F. ) ;
#18662 = EDGE_CURVE ( 'NONE', #5675, #13193, #10597, .T. ) ;
#18663 = CARTESIAN_POINT ( 'NONE',  ( 158.0000000000008527, 125.7007497147323818, 45.00000000000000000 ) ) ;
#18664 = ORIENTED_EDGE ( 'NONE', *, *, #21978, .F. ) ;
#18665 = ORIENTED_EDGE ( 'NONE', *, *, #376, .T. ) ;
#18666 = AXIS2_PLACEMENT_3D ( 'NONE', #25904, #6226, #10828 ) ;
#18667 = EDGE_LOOP ( 'NONE', ( #2806, #3823, #16724, #81 ) ) ;
#18668 = VERTEX_POINT ( 'NONE', #6280 ) ;
#18669 = ORIENTED_EDGE ( 'NONE', *, *, #418, .F. ) ;
#18670 = CARTESIAN_POINT ( 'NONE',  ( -160.0000000000000284, 119.7660240611718905, -22.85081902853004721 ) ) ;
#18671 = DIRECTION ( 'NONE',  ( 0.000000000000000000, 0.000000000000000000, 1.000000000000000000 ) ) ;
#18672 = EDGE_CURVE ( 'NONE', #14862, #11476, #25675, .T. ) ;
#18673 = ADVANCED_FACE ( 'NONE', ( #15200 ), #12485, .F. ) ;
#18674 = DIRECTION ( 'NONE',  ( 1.000000000000000000, -0.000000000000000000, -0.000000000000000000 ) ) ;
#18675 = CARTESIAN_POINT ( 'NONE',  ( 103.3065774809911090, 238.5579845772719239, -26.03670454253122557 ) ) ;
#18676 = LINE ( 'NONE', #27422, #21561 ) ;
#18677 = DIRECTION ( 'NONE',  ( -0.000000000000000000, -0.000000000000000000, -1.000000000000000000 ) ) ;
#18678 = DIRECTION ( 'NONE',  ( 1.000000000000000000, 0.000000000000000000, -0.000000000000000000 ) ) ;
#18679 = VECTOR ( 'NONE', #24286, 1000.000000000000000 ) ;
#18680 = CARTESIAN_POINT ( 'NONE',  ( -207.6571795319446210, 75.48633125953863043, -42.38064732172073690 ) ) ;
#18681 = ADVANCED_FACE ( 'NONE', ( #23814, #21505 ), #8157, .T. ) ;
#18682 = CARTESIAN_POINT ( 'NONE',  ( 110.6543292814727550, 202.4672421913198264, -150.2048413890044003 ) ) ;
#18683 = DIRECTION ( 'NONE',  ( 0.000000000000000000, 0.000000000000000000, -1.000000000000000000 ) ) ;
#18684 = DIRECTION ( 'NONE',  ( 0.8916010070296023216, -0.4528218681377911281, 0.000000000000000000 ) ) ;
#18685 = CARTESIAN_POINT ( 'NONE',  ( -277.2150368962633706, -237.2150368962634559, 105.0000000000000000 ) ) ;
#18686 = EDGE_LOOP ( 'NONE', ( #24917, #3810, #22603, #26344 ) ) ;
#18687 = EDGE_CURVE ( 'NONE', #8486, #1213, #19215, .T. ) ;
#18688 = DIRECTION ( 'NONE',  ( 0.000000000000000000, 0.000000000000000000, -1.000000000000000000 ) ) ;
#18689 = ADVANCED_FACE ( 'NONE', ( #4265 ), #8319, .T. ) ;
#18690 = CARTESIAN_POINT ( 'NONE',  ( 157.4999999999996874, 268.9035626463865469, 45.00000000000000000 ) ) ;
#18691 = VERTEX_POINT ( 'NONE', #19500 ) ;
#18692 = DIRECTION ( 'NONE',  ( 0.000000000000000000, 0.9242245927363030855, 0.3818493186865927203 ) ) ;
#18693 = EDGE_CURVE ( 'NONE', #4982, #22164, #27680, .T. ) ;
#18694 = ORIENTED_EDGE ( 'NONE', *, *, #17384, .F. ) ;
#18695 = ORIENTED_EDGE ( 'NONE', *, *, #15265, .F. ) ;
#18696 = VECTOR ( 'NONE', #27157, 1000.000000000000000 ) ;
#18697 = DIRECTION ( 'NONE',  ( 0.000000000000000000, -1.000000000000000000, 0.000000000000000000 ) ) ;
#18698 = CARTESIAN_POINT ( 'NONE',  ( 157.4999999999998579, 156.0491873085704242, -45.00000000000000000 ) ) ;
#18699 = VERTEX_POINT ( 'NONE', #14630 ) ;
#18700 = VECTOR ( 'NONE', #16634, 1000.000000000000000 ) ;
#18701 = ORIENTED_EDGE ( 'NONE', *, *, #26246, .F. ) ;
#18702 = DIRECTION ( 'NONE',  ( -0.000000000000000000, 0.000000000000000000, -1.000000000000000000 ) ) ;
#18703 = CARTESIAN_POINT ( 'NONE',  ( 92.91655173479981045, 230.8754105999472301, 17.91819147207310792 ) ) ;
#18704 = CARTESIAN_POINT ( 'NONE',  ( -210.0000000000000568, -220.0000000000000853, -90.87829376371895762 ) ) ;
#18706 = EDGE_CURVE ( 'NONE', #10815, #3825, #27566, .T. ) ;
#18705 = ORIENTED_EDGE ( 'NONE', *, *, #8022, .T. ) ;
#18707 = DIRECTION ( 'NONE',  ( 0.000000000000000000, 0.000000000000000000, -1.000000000000000000 ) ) ;
#18708 = ORIENTED_EDGE ( 'NONE', *, *, #12971, .T. ) ;
#18709 = DIRECTION ( 'NONE',  ( -0.000000000000000000, -0.000000000000000000, 1.000000000000000000 ) ) ;
#18710 = CARTESIAN_POINT ( 'NONE',  ( 232.4999999999996305, 83.06687458711267880, 30.86484227207694886 ) ) ;
#18711 = CARTESIAN_POINT ( 'NONE',  ( 119.9999999999999147, 140.0000000000000000, -100.0000000000000142 ) ) ;
#18712 = FACE_OUTER_BOUND ( 'NONE', #23718, .T. ) ;
#18713 = CARTESIAN_POINT ( 'NONE',  ( 157.4999999999998579, 125.9546872184859012, 45.00000000000000000 ) ) ;
#18714 = DIRECTION ( 'NONE',  ( -0.7440215159219103480, -0.6681556583950049033, 0.000000000000000000 ) ) ;
#18715 = CARTESIAN_POINT ( 'NONE',  ( -203.2481855153402250, 92.57460631283319685, -29.78692811926998729 ) ) ;
#18716 = AXIS2_PLACEMENT_3D ( 'NONE', #27130, #6881, #7176 ) ;
#18717 = ORIENTED_EDGE ( 'NONE', *, *, #11274, .F. ) ;
#18718 = DIRECTION ( 'NONE',  ( 0.9960550913260672878, 1.086714821493799823E-17, 0.08873699929240111417 ) ) ;
#18719 = AXIS2_PLACEMENT_3D ( 'NONE', #6344, #8653, #4330 ) ;
#18720 = LINE ( 'NONE', #16574, #15185 ) ;
#18721 = FACE_OUTER_BOUND ( 'NONE', #17999, .T. ) ;
#18722 = DIRECTION ( 'NONE',  ( 0.4528218681383106015, 0.8916010070293384215, -0.000000000000000000 ) ) ;
#18723 = VERTEX_POINT ( 'NONE', #532 ) ;
#18724 = EDGE_CURVE ( 'NONE', #7779, #19503, #17477, .T. ) ;
#18725 = LINE ( 'NONE', #1200, #9600 ) ;
#18726 = EDGE_CURVE ( 'NONE', #15277, #27632, #4540, .T. ) ;
#18727 = ORIENTED_EDGE ( 'NONE', *, *, #11968, .T. ) ;
#18728 = CYLINDRICAL_SURFACE ( 'NONE', #21248, 5.000000000000004441 ) ;
#18729 = CARTESIAN_POINT ( 'NONE',  ( 157.9999999999999147, 213.9842499849850697, 45.00000000000000000 ) ) ;
#18730 = CARTESIAN_POINT ( 'NONE',  ( -273.6211430000234373, -91.18033988749901653, 14.64217782292691261 ) ) ;
#18731 = ORIENTED_EDGE ( 'NONE', *, *, #3963, .T. ) ;
#18732 = DIRECTION ( 'NONE',  ( 0.4528218681381301347, -0.8916010070294301260, 0.000000000000000000 ) ) ;
#18733 = EDGE_LOOP ( 'NONE', ( #22313, #12460, #4207, #15826 ) ) ;
#18734 = LINE ( 'NONE', #18323, #20788 ) ;
#18735 = AXIS2_PLACEMENT_3D ( 'NONE', #1519, #3243, #10151 ) ;
#18736 = CARTESIAN_POINT ( 'NONE',  ( 109.9737507963278773, 258.9420169438926678, 43.16738424200269719 ) ) ;
#18737 = ORIENTED_EDGE ( 'NONE', *, *, #9301, .F. ) ;
#18738 = ORIENTED_EDGE ( 'NONE', *, *, #757, .T. ) ;
#18739 = DIRECTION ( 'NONE',  ( 0.000000000000000000, -1.000000000000000000, 0.000000000000000000 ) ) ;
#18740 = ORIENTED_EDGE ( 'NONE', *, *, #24717, .F. ) ;
#18741 = AXIS2_PLACEMENT_3D ( 'NONE', #2243, #15487, #4120 ) ;
#18742 = ADVANCED_FACE ( 'NONE', ( #17909 ), #15486, .F. ) ;
#18743 = VERTEX_POINT ( 'NONE', #24371 ) ;
#18744 = ORIENTED_EDGE ( 'NONE', *, *, #20699, .F. ) ;
#18745 = DIRECTION ( 'NONE',  ( 1.049727191138617586E-16, 0.5150380749100552658, -0.8571673007021115565 ) ) ;
#18746 = EDGE_CURVE ( 'NONE', #12495, #11481, #18872, .T. ) ;
#18747 = DIRECTION ( 'NONE',  ( 1.000000000000000000, 2.312964634635742957E-16, 0.000000000000000000 ) ) ;
#18748 = DIRECTION ( 'NONE',  ( -1.000000000000000000, -0.000000000000000000, -0.000000000000000000 ) ) ;
#18749 = DIRECTION ( 'NONE',  ( 1.000000000000000000, -0.000000000000000000, -0.000000000000000000 ) ) ;
#18750 = CYLINDRICAL_SURFACE ( 'NONE', #27775, 10.00000000000000888 ) ;
#18751 = PLANE ( 'NONE',  #8826 ) ;
#18752 = VECTOR ( 'NONE', #11384, 1000.000000000000000 ) ;
#18753 = DIRECTION ( 'NONE',  ( -1.000000000000000000, 0.000000000000000000, 0.000000000000000000 ) ) ;
#18754 = EDGE_CURVE ( 'NONE', #12868, #18572, #17626, .T. ) ;
#18755 = DIRECTION ( 'NONE',  ( -0.9611633748070274041, -0.2759800118297804916, -0.000000000000000000 ) ) ;
#18756 = DIRECTION ( 'NONE',  ( -1.000000000000000000, 0.000000000000000000, 0.000000000000000000 ) ) ;
#18757 = CARTESIAN_POINT ( 'NONE',  ( -217.2892621185082760, 109.4029876883478352, -15.00000000000000000 ) ) ;
#18758 = EDGE_LOOP ( 'NONE', ( #11296, #17186 ) ) ;
#18759 = ADVANCED_FACE ( 'NONE', ( #8723 ), #4403, .F. ) ;
#18760 = CARTESIAN_POINT ( 'NONE',  ( -8.284241264067754074, 132.5788630569019233, 15.89734390185955171 ) ) ;
#18761 = AXIS2_PLACEMENT_3D ( 'NONE', #3446, #3725, #25562 ) ;
#18762 = ADVANCED_FACE ( 'NONE', ( #6989 ), #4827, .F. ) ;
#18763 = CIRCLE ( 'NONE', #10052, 30.00000000000000355 ) ;
#18764 = FACE_OUTER_BOUND ( 'NONE', #26424, .T. ) ;
#18765 = CARTESIAN_POINT ( 'NONE',  ( 186.0596930950812293, 94.49506802741289846, -45.00000000000000000 ) ) ;
#18766 = FILL_AREA_STYLE ('',( #5549 ) ) ;
#18767 = FACE_OUTER_BOUND ( 'NONE', #18686, .T. ) ;
#18768 = ORIENTED_EDGE ( 'NONE', *, *, #28086, .F. ) ;
#18769 = AXIS2_PLACEMENT_3D ( 'NONE', #5488, #25308, #16557 ) ;
#18770 = LINE ( 'NONE', #25232, #17115 ) ;
#18771 = ORIENTED_EDGE ( 'NONE', *, *, #9594, .T. ) ;
#18772 = DIRECTION ( 'NONE',  ( -0.000000000000000000, -0.000000000000000000, -1.000000000000000000 ) ) ;
#18773 = ORIENTED_EDGE ( 'NONE', *, *, #24507, .F. ) ;
#18774 = ORIENTED_EDGE ( 'NONE', *, *, #4077, .T. ) ;
#18775 = AXIS2_PLACEMENT_3D ( 'NONE', #15171, #21903, #9115 ) ;
#18776 = VECTOR ( 'NONE', #6413, 1000.000000000000000 ) ;
#18777 = ORIENTED_EDGE ( 'NONE', *, *, #17716, .T. ) ;
#18778 = ORIENTED_EDGE ( 'NONE', *, *, #1378, .T. ) ;
#18779 = CARTESIAN_POINT ( 'NONE',  ( 114.1093725872595854, 228.3710704777231797, 98.08429852854952458 ) ) ;
#18780 = CARTESIAN_POINT ( 'NONE',  ( 175.6862808370088089, 157.7720269260891826, -45.00000000000000000 ) ) ;
#18781 = CARTESIAN_POINT ( 'NONE',  ( -210.3420575078734771, -220.0000000000000284, -91.10584728836482782 ) ) ;
#18782 = CIRCLE ( 'NONE', #6392, 6.000000000000005329 ) ;
#18783 = CARTESIAN_POINT ( 'NONE',  ( -148.7315380569646379, 124.1728174158764517, -19.50986539812211618 ) ) ;
#18784 = AXIS2_PLACEMENT_3D ( 'NONE', #12085, #5319, #16529 ) ;
#18785 = DIRECTION ( 'NONE',  ( -0.9506505318133474658, 0.3102637045530776683, 0.000000000000000000 ) ) ;
#18786 = DIRECTION ( 'NONE',  ( -0.5457381880580551847, 0.8379557447115634217, 0.000000000000000000 ) ) ;
#18787 = EDGE_CURVE ( 'NONE', #11545, #13481, #22365, .T. ) ;
#18788 = DIRECTION ( 'NONE',  ( 1.321694076934710155E-16, -1.000000000000000000, 0.000000000000000000 ) ) ;
#18789 = DIRECTION ( 'NONE',  ( 0.000000000000000000, 0.000000000000000000, -1.000000000000000000 ) ) ;
#18790 = CARTESIAN_POINT ( 'NONE',  ( -207.6837665628285663, 89.33788410654877055, 27.01424684382055830 ) ) ;
#18791 = PLANE ( 'NONE',  #957 ) ;
#18792 = CARTESIAN_POINT ( 'NONE',  ( 112.5248869502488986, 215.0130877889307044, 45.00000000000000000 ) ) ;
#18793 = CARTESIAN_POINT ( 'NONE',  ( 144.9999999999998863, 220.0000000000000284, 109.9999999999999858 ) ) ;
#18794 = ORIENTED_EDGE ( 'NONE', *, *, #12535, .T. ) ;
#18795 = AXIS2_PLACEMENT_3D ( 'NONE', #1858, #23854, #15528 ) ;
#18796 = EDGE_CURVE ( 'NONE', #9114, #9224, #11025, .T. ) ;
#18797 = CARTESIAN_POINT ( 'NONE',  ( -34.12965183067004205, -18.01420295945611727, 100.0000000000000000 ) ) ;
#18798 = DIRECTION ( 'NONE',  ( 1.321694076934710155E-16, -1.000000000000000000, 0.000000000000000000 ) ) ;
#18800 = ORIENTED_EDGE ( 'NONE', *, *, #6731, .F. ) ;
#18799 = VERTEX_POINT ( 'NONE', #9295 ) ;
#18801 = AXIS2_PLACEMENT_3D ( 'NONE', #24953, #821, #22225 ) ;
#18802 = EDGE_CURVE ( 'NONE', #13277, #9020, #6568, .T. ) ;
#18803 = DIRECTION ( 'NONE',  ( 0.9985600561963485777, 0.05364526231779760679, 0.000000000000000000 ) ) ;
#18804 = ORIENTED_EDGE ( 'NONE', *, *, #23231, .F. ) ;
#18805 = ORIENTED_EDGE ( 'NONE', *, *, #23843, .T. ) ;
#18806 = ORIENTED_EDGE ( 'NONE', *, *, #11591, .T. ) ;
#18807 = EDGE_LOOP ( 'NONE', ( #19017, #26261, #8202, #2652 ) ) ;
#18808 = ORIENTED_EDGE ( 'NONE', *, *, #21111, .F. ) ;
#18809 = ORIENTED_EDGE ( 'NONE', *, *, #9496, .F. ) ;
#18810 = CARTESIAN_POINT ( 'NONE',  ( 33.10302365956999182, 203.2034914284457159, 12.99999999999999822 ) ) ;
#18811 = AXIS2_PLACEMENT_3D ( 'NONE', #4114, #21644, #1956 ) ;
#18812 = DIRECTION ( 'NONE',  ( 1.000000000000000000, -0.000000000000000000, -0.000000000000000000 ) ) ;
#18813 = CARTESIAN_POINT ( 'NONE',  ( 109.8052436612091469, 255.9788950837981645, -41.51592141934425229 ) ) ;
#18814 = VECTOR ( 'NONE', #1483, 1000.000000000000000 ) ;
#18815 = CARTESIAN_POINT ( 'NONE',  ( 217.4999999999996305, 494.4107529906318632, 100.0000000000000142 ) ) ;
#18816 = EDGE_CURVE ( 'NONE', #3560, #4902, #249, .T. ) ;
#18817 = DIRECTION ( 'NONE',  ( 0.000000000000000000, 0.000000000000000000, 1.000000000000000000 ) ) ;
#18818 = LINE ( 'NONE', #8184, #15099 ) ;
#18819 = CARTESIAN_POINT ( 'NONE',  ( -214.2384622483376688, 55.08766841006207926, -45.11431866370089239 ) ) ;
#18820 = CARTESIAN_POINT ( 'NONE',  ( 157.9999999999998010, 236.5551250525490161, 45.00000000000000000 ) ) ;
#18821 = CARTESIAN_POINT ( 'NONE',  ( -17.24491960465745777, 0.000000000000000000, 95.00000000000000000 ) ) ;
#18822 = DIRECTION ( 'NONE',  ( -0.000000000000000000, -0.000000000000000000, -1.000000000000000000 ) ) ;
#18823 = CARTESIAN_POINT ( 'NONE',  ( 134.9999999999998579, 455.5353319318992362, -162.9307281190808681 ) ) ;
#18824 = VERTEX_POINT ( 'NONE', #9007 ) ;
#18825 = CARTESIAN_POINT ( 'NONE',  ( -196.7149000058354602, 98.38617570187021499, 31.27679534840562781 ) ) ;
#18826 = EDGE_CURVE ( 'NONE', #11076, #17424, #17762, .T. ) ;
#18827 = CIRCLE ( 'NONE', #26612, 5.000000000000004441 ) ;
#18828 = EDGE_CURVE ( 'NONE', #1725, #16686, #24367, .T. ) ;
#18829 = DIRECTION ( 'NONE',  ( 0.000000000000000000, 1.000000000000000000, 0.000000000000000000 ) ) ;
#18830 = VERTEX_POINT ( 'NONE', #22220 ) ;
#18831 = CARTESIAN_POINT ( 'NONE',  ( 0.000000000000000000, 0.000000000000000000, 0.000000000000000000 ) ) ;
#18832 = ORIENTED_EDGE ( 'NONE', *, *, #10100, .F. ) ;
#18833 = ORIENTED_EDGE ( 'NONE', *, *, #3639, .F. ) ;
#18834 = AXIS2_PLACEMENT_3D ( 'NONE', #9156, #15778, #2111 ) ;
#18835 = LINE ( 'NONE', #14965, #9722 ) ;
#18836 = DIRECTION ( 'NONE',  ( -0.000000000000000000, -0.000000000000000000, -1.000000000000000000 ) ) ;
#18837 = ORIENTED_EDGE ( 'NONE', *, *, #2155, .F. ) ;
#18839 = EDGE_CURVE ( 'NONE', #8538, #2906, #993, .T. ) ;
#18838 = VERTEX_POINT ( 'NONE', #24663 ) ;
#18840 = LINE ( 'NONE', #14541, #14103 ) ;
#18841 = EDGE_CURVE ( 'NONE', #26462, #12700, #2383, .T. ) ;
#18842 = CARTESIAN_POINT ( 'NONE',  ( -146.6428522700808230, 17.24192588826928585, 80.00000000000001421 ) ) ;
#18843 = DIRECTION ( 'NONE',  ( 0.5457381880580733924, 0.8379557447115515423, 0.000000000000000000 ) ) ;
#18844 = ORIENTED_EDGE ( 'NONE', *, *, #22426, .F. ) ;
#18845 = CARTESIAN_POINT ( 'NONE',  ( -277.2150368962633706, -237.2150368962634559, -94.99999999999985789 ) ) ;
#18846 = ORIENTED_EDGE ( 'NONE', *, *, #3152, .T. ) ;
#18847 = CARTESIAN_POINT ( 'NONE',  ( -63.57415822541634043, 29.64876300893806516, 100.0000000000000000 ) ) ;
#18848 = AXIS2_PLACEMENT_3D ( 'NONE', #11565, #22467, #25049 ) ;
#18849 = LINE ( 'NONE', #27319, #2553 ) ;
#18850 = EDGE_CURVE ( 'NONE', #19026, #17930, #13850, .T. ) ;
#18851 = CARTESIAN_POINT ( 'NONE',  ( 157.9999999999997442, 251.0945000900840398, 45.00000000000000000 ) ) ;
#18852 = LINE ( 'NONE', #7800, #4861 ) ;
#18853 = FACE_OUTER_BOUND ( 'NONE', #2432, .T. ) ;
#18854 = FACE_OUTER_BOUND ( 'NONE', #7106, .T. ) ;
#18855 = CIRCLE ( 'NONE', #26191, 10.70611877156249214 ) ;
#18856 = CARTESIAN_POINT ( 'NONE',  ( 161.6393910565651026, 206.2021604053517763, -150.8447356795924179 ) ) ;
#18857 = ORIENTED_EDGE ( 'NONE', *, *, #28176, .T. ) ;
#18858 = CARTESIAN_POINT ( 'NONE',  ( 134.9999999999998579, -150.0000000000000284, 84.99999999999995737 ) ) ;
#18859 = DIRECTION ( 'NONE',  ( 1.000000000000000000, 0.000000000000000000, -0.000000000000000000 ) ) ;
#18860 = CARTESIAN_POINT ( 'NONE',  ( 158.0000000000005400, 158.3031248123239436, -45.00000000000000000 ) ) ;
#18861 = CARTESIAN_POINT ( 'NONE',  ( -210.0000000000000568, -157.0000000000000284, -110.0000000000000284 ) ) ;
#18862 = ORIENTED_EDGE ( 'NONE', *, *, #27579, .F. ) ;
#18863 = PLANE ( 'NONE',  #14640 ) ;
#18864 = EDGE_LOOP ( 'NONE', ( #26718, #3677, #14991, #5983 ) ) ;
#18865 = FACE_OUTER_BOUND ( 'NONE', #3819, .T. ) ;
#18866 = DIRECTION ( 'NONE',  ( 0.000000000000000000, 0.000000000000000000, -1.000000000000000000 ) ) ;
#18867 = DIRECTION ( 'NONE',  ( -0.7440215159218956931, 0.6681556583950213346, 0.000000000000000000 ) ) ;
#18868 = ORIENTED_EDGE ( 'NONE', *, *, #8314, .F. ) ;
#18869 = CARTESIAN_POINT ( 'NONE',  ( 158.0000000000012221, 90.59049960963380954, -45.00000000000000000 ) ) ;
#18870 = LINE ( 'NONE', #7959, #13435 ) ;
#18871 = ORIENTED_EDGE ( 'NONE', *, *, #12122, .T. ) ;
#18872 = CIRCLE ( 'NONE', #6483, 22.49999999999997868 ) ;
#18873 = LINE ( 'NONE', #23328, #21645 ) ;
#18874 = CARTESIAN_POINT ( 'NONE',  ( 142.6536686473019699, 201.5224093497741649, 45.00000000000000000 ) ) ;
#18875 = ORIENTED_EDGE ( 'NONE', *, *, #24097, .T. ) ;
#18876 = VECTOR ( 'NONE', #14155, 1000.000000000000114 ) ;
#18877 = ORIENTED_EDGE ( 'NONE', *, *, #18162, .F. ) ;
#18878 = CARTESIAN_POINT ( 'NONE',  ( 282.4999999999996589, 19.41075299063184900, 87.99671038392668265 ) ) ;
#18879 = ORIENTED_EDGE ( 'NONE', *, *, #15463, .T. ) ;
#18880 = AXIS2_PLACEMENT_3D ( 'NONE', #5125, #25230, #12036 ) ;
#18881 = VERTEX_POINT ( 'NONE', #20057 ) ;
#18882 = ORIENTED_EDGE ( 'NONE', *, *, #8931, .F. ) ;
#18883 = AXIS2_PLACEMENT_3D ( 'NONE', #7096, #9404, #777 ) ;
#18884 = DIRECTION ( 'NONE',  ( 0.000000000000000000, -1.000000000000000000, 0.000000000000000000 ) ) ;
#18885 = ADVANCED_FACE ( 'NONE', ( #9151 ), #19832, .T. ) ;
#18886 = CARTESIAN_POINT ( 'NONE',  ( 109.9999999999998863, 330.0000000000000000, 100.0000000000000142 ) ) ;
#18887 = EDGE_CURVE ( 'NONE', #25689, #19223, #5400, .T. ) ;
#18888 = CARTESIAN_POINT ( 'NONE',  ( -71.37541315349507443, 150.2892445414773590, -5.000000000000004441 ) ) ;
#18889 = B_SPLINE_CURVE_WITH_KNOTS ( 'NONE', 3,
 ( #9852, #20760, #14172, #24512, #16049, #24655, #4820, #20485, #26809 ),
 .UNSPECIFIED., .F., .F.,
 ( 4, 2, 1, 2, 4 ),
 ( 0.000000000000000000, 0.003993085574633946713, 0.007986171149267893427, 0.01197925672390184014, 0.01597234229853578685 ),
 .UNSPECIFIED. ) ;
#18890 = LINE ( 'NONE', #8261, #14723 ) ;
#18891 = LINE ( 'NONE', #19736, #732 ) ;
#18892 = DIRECTION ( 'NONE',  ( -0.000000000000000000, -0.000000000000000000, -1.000000000000000000 ) ) ;
#18893 = CIRCLE ( 'NONE', #2374, 19.07743405327024888 ) ;
#18894 = DIRECTION ( 'NONE',  ( -0.8916010070298868717, -0.4528218681372309651, 0.000000000000000000 ) ) ;
#18895 = DIRECTION ( 'NONE',  ( 0.4528218681377311206, 0.8916010070296327417, -0.000000000000000000 ) ) ;
#18897 = DIRECTION ( 'NONE',  ( 0.000000000000000000, 0.000000000000000000, -1.000000000000000000 ) ) ;
#18896 = AXIS2_PLACEMENT_3D ( 'NONE', #24178, #13267, #22016 ) ;
#18898 = DIRECTION ( 'NONE',  ( 1.000000000000000000, 0.000000000000000000, 0.000000000000000000 ) ) ;
#18899 = ORIENTED_EDGE ( 'NONE', *, *, #26457, .F. ) ;
#18900 = CARTESIAN_POINT ( 'NONE',  ( 158.0000000000009379, 118.1771246922112653, 45.00000000000000000 ) ) ;
#18901 = VECTOR ( 'NONE', #15030, 1000.000000000000000 ) ;
#18902 = CARTESIAN_POINT ( 'NONE',  ( 109.3254858558567122, 254.7367570746976639, -35.86634952330716430 ) ) ;
#18903 = LINE ( 'NONE', #27370, #14910 ) ;
#18904 = CARTESIAN_POINT ( 'NONE',  ( 134.9999999999998579, 220.0000000000000284, -99.00000000000001421 ) ) ;
#18905 = LINE ( 'NONE', #3814, #17074 ) ;
#18906 = ORIENTED_EDGE ( 'NONE', *, *, #16066, .T. ) ;
#18907 = DIRECTION ( 'NONE',  ( 0.000000000000000000, -1.000000000000000000, 0.000000000000000000 ) ) ;
#18908 = ORIENTED_EDGE ( 'NONE', *, *, #8250, .F. ) ;
#18909 = EDGE_CURVE ( 'NONE', #19721, #18983, #16139, .T. ) ;
#18910 = FACE_OUTER_BOUND ( 'NONE', #513, .T. ) ;
#18911 = VERTEX_POINT ( 'NONE', #16336 ) ;
#18912 = SHAPE_REPRESENTATION ( 'Drive Gear', ( #10637 ), #19371 ) ;
#18913 = ORIENTED_EDGE ( 'NONE', *, *, #17253, .F. ) ;
#18914 = CARTESIAN_POINT ( 'NONE',  ( -42.53273978471833061, 130.9733465240572343, 14.93735646117641913 ) ) ;
#18915 = CIRCLE ( 'NONE', #14802, 16.36034929305424512 ) ;
#18916 = ORIENTED_EDGE ( 'NONE', *, *, #3310, .T. ) ;
#18917 = EDGE_CURVE ( 'NONE', #25403, #21137, #1231, .T. ) ;
#18918 = VERTEX_POINT ( 'NONE', #16609 ) ;
#18919 = AXIS2_PLACEMENT_3D ( 'NONE', #9292, #2521, #18056 ) ;
#18920 = CYLINDRICAL_SURFACE ( 'NONE', #11813, 49.99999999999998579 ) ;
#18921 = DIRECTION ( 'NONE',  ( 0.000000000000000000, -0.000000000000000000, 1.000000000000000000 ) ) ;
#18922 = DIRECTION ( 'NONE',  ( 1.000000000000000000, 0.000000000000000000, 0.000000000000000000 ) ) ;
#18923 = EDGE_CURVE ( 'NONE', #1393, #2012, #17026, .T. ) ;
#18924 = CIRCLE ( 'NONE', #3781, 5.000000000000004441 ) ;
#18925 = EDGE_CURVE ( 'NONE', #12219, #5230, #18346, .T. ) ;
#18926 = EDGE_CURVE ( 'NONE', #14569, #10474, #22932, .T. ) ;
#18927 = CARTESIAN_POINT ( 'NONE',  ( -137.3782106177114883, 129.0617887715208951, -17.02469355150050845 ) ) ;
#18928 = DIRECTION ( 'NONE',  ( 0.000000000000000000, -1.000000000000000000, 0.000000000000000000 ) ) ;
#18929 = CARTESIAN_POINT ( 'NONE',  ( -63.57415822541634043, 75.97823757117562593, 95.00000000000000000 ) ) ;
#18930 = CARTESIAN_POINT ( 'NONE',  ( -270.6423355020924646, -165.1562042664794774, 88.05640019106880345 ) ) ;
#18931 = CARTESIAN_POINT ( 'NONE',  ( 157.4999999999998295, 226.2696875187675118, 45.00000000000000000 ) ) ;
#18932 = CARTESIAN_POINT ( 'NONE',  ( -107.3221550338875687, 69.54464929955099706, 83.00000000000001421 ) ) ;
#18933 = DIRECTION ( 'NONE',  ( -1.000000000000000000, 0.000000000000000000, 3.074769666655405408E-15 ) ) ;
#18934 = FACE_OUTER_BOUND ( 'NONE', #5862, .T. ) ;
#18935 = CARTESIAN_POINT ( 'NONE',  ( 217.4999999999996305, 83.06687458711267880, 30.86484227207694886 ) ) ;
#18936 = ORIENTED_EDGE ( 'NONE', *, *, #9551, .T. ) ;
#18937 = CIRCLE ( 'NONE', #14354, 5.999999999999977796 ) ;
#18938 = CIRCLE ( 'NONE', #4715, 2.000000000000000000 ) ;
#18939 = DIRECTION ( 'NONE',  ( -0.8916010070294301260, -0.4528218681381301347, 0.000000000000000000 ) ) ;
#18940 = CARTESIAN_POINT ( 'NONE',  ( 106.6069624357703134, 210.3128146450298743, -143.4408232581956213 ) ) ;
#18941 = AXIS2_PLACEMENT_3D ( 'NONE', #3516, #14175, #20488 ) ;
#18943 = ORIENTED_EDGE ( 'NONE', *, *, #6435, .T. ) ;
#18942 = ORIENTED_EDGE ( 'NONE', *, *, #4470, .F. ) ;
#18944 = VECTOR ( 'NONE', #964, 1000.000000000000000 ) ;
#18945 = LINE ( 'NONE', #10186, #7474 ) ;
#18946 = ORIENTED_EDGE ( 'NONE', *, *, #22268, .T. ) ;
#18947 = VERTEX_POINT ( 'NONE', #5686 ) ;
#18948 = VERTEX_POINT ( 'NONE', #7838 ) ;
#18949 = EDGE_CURVE ( 'NONE', #24145, #14477, #9445, .T. ) ;
#18950 = ADVANCED_FACE ( 'NONE', ( #14457 ), #25221, .F. ) ;
#18951 = VERTEX_POINT ( 'NONE', #18617 ) ;
#18952 = ORIENTED_EDGE ( 'NONE', *, *, #22325, .F. ) ;
#18953 = ORIENTED_EDGE ( 'NONE', *, *, #26759, .T. ) ;
#18954 = VECTOR ( 'NONE', #25454, 1000.000000000000000 ) ;
#18955 = FACE_OUTER_BOUND ( 'NONE', #21093, .T. ) ;
#18956 = TOROIDAL_SURFACE ( 'NONE', #23086, 23.59849023212046859, 2.000000000000000000 ) ;
#18957 = EDGE_CURVE ( 'NONE', #23507, #23933, #7283, .T. ) ;
#18958 = CARTESIAN_POINT ( 'NONE',  ( 157.4999999999998579, 113.4153121809506786, 45.00000000000000000 ) ) ;
#18959 = AXIS2_PLACEMENT_3D ( 'NONE', #10748, #21370, #10886 ) ;
#18960 = CARTESIAN_POINT ( 'NONE',  ( 109.9878487949967791, 258.9938397943334962, -44.12861322695685118 ) ) ;
#18961 = CARTESIAN_POINT ( 'NONE',  ( -3.658769994963756211, 132.7364076050659492, -15.88886450207448853 ) ) ;
#18962 = CARTESIAN_POINT ( 'NONE',  ( 8.415662294793918363, -4.274104551145060604, 45.00000000000000000 ) ) ;
#18963 = CARTESIAN_POINT ( 'NONE',  ( 158.0000000000013642, 78.05112457209858690, 45.00000000000000000 ) ) ;
#18964 = LINE ( 'NONE', #27707, #13430 ) ;
#18965 = CARTESIAN_POINT ( 'NONE',  ( 109.4170858023077244, 204.3262714183213689, -139.0380470571626859 ) ) ;
#18966 = CYLINDRICAL_SURFACE ( 'NONE', #7754, 5.000000000000004441 ) ;
#18967 = LINE ( 'NONE', #3585, #21149 ) ;
#18968 = DIRECTION ( 'NONE',  ( -1.000000000000000000, 0.000000000000000000, 0.000000000000000000 ) ) ;
#18969 = ORIENTED_EDGE ( 'NONE', *, *, #23480, .T. ) ;
#18970 = AXIS2_PLACEMENT_3D ( 'NONE', #17259, #19274, #28019 ) ;
#18971 = LINE ( 'NONE', #12666, #9163 ) ;
#18972 = PRODUCT ( 'Drill Stand and Mount', 'Drill Stand and Mount', '', ( #11824 ) ) ;
#18973 = CARTESIAN_POINT ( 'NONE',  ( 157.9999999999998295, 224.0157500150140208, -45.00000000000000000 ) ) ;
#18974 = ORIENTED_EDGE ( 'NONE', *, *, #6976, .F. ) ;
#18975 = DIRECTION ( 'NONE',  ( 0.000000000000000000, -1.000000000000000000, 1.387778780781445429E-16 ) ) ;
#18976 = AXIS2_PLACEMENT_3D ( 'NONE', #10145, #14180, #20634 ) ;
#18977 = VERTEX_POINT ( 'NONE', #16056 ) ;
#18978 = VERTEX_POINT ( 'NONE', #24947 ) ;
#18979 = EDGE_CURVE ( 'NONE', #800, #20034, #5262, .T. ) ;
#18980 = LINE ( 'NONE', #3459, #996 ) ;
#18981 = DIRECTION ( 'NONE',  ( 0.000000000000000000, -1.000000000000000000, 0.000000000000000000 ) ) ;
#18982 = ORIENTED_EDGE ( 'NONE', *, *, #23762, .T. ) ;
#18983 = VERTEX_POINT ( 'NONE', #16471 ) ;
#18984 = PLANE ( 'NONE',  #1700 ) ;
#18985 = CARTESIAN_POINT ( 'NONE',  ( 109.8052321039920685, 255.9787816365463016, 41.51582300832603067 ) ) ;
#18986 = PLANE ( 'NONE',  #26543 ) ;
#18987 = ORIENTED_EDGE ( 'NONE', *, *, #831, .F. ) ;
#18988 = DIRECTION ( 'NONE',  ( 1.321694076934710155E-16, -1.000000000000000000, 0.000000000000000000 ) ) ;
#18989 = ORIENTED_EDGE ( 'NONE', *, *, #25428, .F. ) ;
#18990 = AXIS2_PLACEMENT_3D ( 'NONE', #18088, #16084, #22389 ) ;
#18991 = CARTESIAN_POINT ( 'NONE',  ( -56.02075117275366978, 110.3042093914830559, 45.00000000000000000 ) ) ;
#18992 = EDGE_CURVE ( 'NONE', #21166, #10546, #21470, .T. ) ;
#18993 = EDGE_CURVE ( 'NONE', #8245, #9774, #25922, .T. ) ;
#18994 = DIRECTION ( 'NONE',  ( 0.8916010070300078860, -0.4528218681369923782, 0.000000000000000000 ) ) ;
#18995 = DIRECTION ( 'NONE',  ( -0.8142945039115421224, -0.5804519453834706688, 0.000000000000000000 ) ) ;
#18996 = LINE ( 'NONE', #25320, #26879 ) ;
#18997 = VECTOR ( 'NONE', #18271, 999.9999999999998863 ) ;
#18998 = DIRECTION ( 'NONE',  ( 1.000000000000000000, 0.000000000000000000, 0.000000000000000000 ) ) ;
#18999 = DIRECTION ( 'NONE',  ( -1.000000000000000000, 0.000000000000000000, -2.220446049250266932E-15 ) ) ;
#19000 = LINE ( 'NONE', #8225, #22502 ) ;
#19001 = VERTEX_POINT ( 'NONE', #27921 ) ;
#19002 = CARTESIAN_POINT ( 'NONE',  ( 79.99999999999991473, 110.0000000000000142, 100.0000000000000000 ) ) ;
#19003 = FACE_OUTER_BOUND ( 'NONE', #18598, .T. ) ;
#19004 = DIRECTION ( 'NONE',  ( -0.000000000000000000, -0.000000000000000000, -1.000000000000000000 ) ) ;
#19005 = CARTESIAN_POINT ( 'NONE',  ( 157.9999999999997442, 256.1102501050980322, -45.00000000000000000 ) ) ;
#19006 = EDGE_LOOP ( 'NONE', ( #19009, #12138, #9170, #22733 ) ) ;
#19007 = ADVANCED_FACE ( 'NONE', ( #28207 ), #19038, .F. ) ;
#19008 = DIRECTION ( 'NONE',  ( -0.000000000000000000, -0.000000000000000000, 1.000000000000000000 ) ) ;
#19009 = ORIENTED_EDGE ( 'NONE', *, *, #15420, .F. ) ;
#19010 = ADVANCED_FACE ( 'NONE', ( #7981 ), #14594, .F. ) ;
#19011 = DIRECTION ( 'NONE',  ( 1.000000000000000000, 1.530283246943720628E-16, 0.000000000000000000 ) ) ;
#19012 = DIRECTION ( 'NONE',  ( -0.000000000000000000, 0.000000000000000000, -1.000000000000000000 ) ) ;
#19013 = CARTESIAN_POINT ( 'NONE',  ( -223.7492756146818067, 88.78109556843006089, 14.68106835128092946 ) ) ;
#19014 = ORIENTED_EDGE ( 'NONE', *, *, #3921, .T. ) ;
#19015 = DIRECTION ( 'NONE',  ( -1.000000000000000000, -0.000000000000000000, 0.000000000000000000 ) ) ;
#19016 = DIRECTION ( 'NONE',  ( -0.000000000000000000, 0.000000000000000000, -1.000000000000000000 ) ) ;
#19017 = ORIENTED_EDGE ( 'NONE', *, *, #19565, .T. ) ;
#19018 = AXIS2_PLACEMENT_3D ( 'NONE', #25878, #27876, #8220 ) ;
#19019 = FACE_OUTER_BOUND ( 'NONE', #11185, .T. ) ;
#19020 = CARTESIAN_POINT ( 'NONE',  ( 109.9999999999999005, 260.0000000000000000, 45.00000000000000000 ) ) ;
#19021 = VERTEX_POINT ( 'NONE', #6105 ) ;
#19022 = ORIENTED_EDGE ( 'NONE', *, *, #830, .T. ) ;
#19023 = LINE ( 'NONE', #16595, #13167 ) ;
#19024 = ORIENTED_EDGE ( 'NONE', *, *, #26101, .T. ) ;
#19025 = ORIENTED_EDGE ( 'NONE', *, *, #16104, .T. ) ;
#19026 = VERTEX_POINT ( 'NONE', #25777 ) ;
#19027 = DIRECTION ( 'NONE',  ( 0.000000000000000000, 0.000000000000000000, 1.000000000000000000 ) ) ;
#19028 = EDGE_CURVE ( 'NONE', #14759, #83, #12309, .T. ) ;
#19029 = EDGE_CURVE ( 'NONE', #6262, #18388, #23350, .T. ) ;
#19030 = CARTESIAN_POINT ( 'NONE',  ( -210.0000000000000568, -220.0000000000000853, 109.1217062362809145 ) ) ;
#19031 = FACE_OUTER_BOUND ( 'NONE', #15176, .T. ) ;
#19032 = VECTOR ( 'NONE', #6733, 1000.000000000000000 ) ;
#19033 = LINE ( 'NONE', #14880, #14253 ) ;
#19034 = CARTESIAN_POINT ( 'NONE',  ( -273.6211430000234373, -91.18033988749901653, 14.64217782292691261 ) ) ;
#19035 = CARTESIAN_POINT ( 'NONE',  ( -231.1655399901031842, 65.02775169231905750, -6.844214734956196367 ) ) ;
#19036 = DIRECTION ( 'NONE',  ( 0.000000000000000000, -9.486769009248163798E-17, 1.000000000000000000 ) ) ;
#19037 = VECTOR ( 'NONE', #1484, 1000.000000000000000 ) ;
#19038 = PLANE ( 'NONE',  #21619 ) ;
#19039 = CARTESIAN_POINT ( 'NONE',  ( 153.4775906502256930, 212.3463313526982859, 45.00000000000000000 ) ) ;
#19040 = CARTESIAN_POINT ( 'NONE',  ( -70.31278697424053803, 101.4626071723526195, -145.0000000000000000 ) ) ;
#19041 = ORIENTED_EDGE ( 'NONE', *, *, #24565, .T. ) ;
#19042 = EDGE_CURVE ( 'NONE', #19942, #19398, #1512, .T. ) ;
#19043 = CARTESIAN_POINT ( 'NONE',  ( 154.4185842870419663, 232.3660254037841639, 45.00000000000000000 ) ) ;
#19044 = CARTESIAN_POINT ( 'NONE',  ( 109.5784524905024853, 255.7787112550930999, -37.67977400422613243 ) ) ;
#19045 = LINE ( 'NONE', #25228, #20864 ) ;
#19046 = DIRECTION ( 'NONE',  ( 0.7071067811865474617, 0.000000000000000000, -0.7071067811865474617 ) ) ;
#19047 = VERTEX_POINT ( 'NONE', #21047 ) ;
#19048 = ADVANCED_FACE ( 'NONE', ( #3807 ), #12730, .F. ) ;
#19049 = ADVANCED_FACE ( 'NONE', ( #17300 ), #28063, .F. ) ;
#19050 = DIRECTION ( 'NONE',  ( 1.000000000000000000, 0.000000000000000000, 0.000000000000000000 ) ) ;
#19051 = ORIENTED_EDGE ( 'NONE', *, *, #25300, .T. ) ;
#19052 = CARTESIAN_POINT ( 'NONE',  ( 157.4999999999998579, 68.27356204582390831, 45.00000000000000000 ) ) ;
#19053 = VERTEX_POINT ( 'NONE', #16883 ) ;
#19054 = VECTOR ( 'NONE', #19531, 999.9999999999998863 ) ;
#19055 = ADVANCED_FACE ( 'NONE', ( #21332 ), #5819, .F. ) ;
#19056 = AXIS2_PLACEMENT_3D ( 'NONE', #24806, #9720, #13907 ) ;
#19057 = ORIENTED_EDGE ( 'NONE', *, *, #18050, .T. ) ;
#19058 = CARTESIAN_POINT ( 'NONE',  ( -97.96203580167062341, 136.1557472209292143, 13.53404630376955176 ) ) ;
#19059 = ORIENTED_EDGE ( 'NONE', *, *, #14231, .T. ) ;
#19060 = VECTOR ( 'NONE', #150, 1000.000000000000000 ) ;
#19061 = VERTEX_POINT ( 'NONE', #10282 ) ;
#19062 = DIRECTION ( 'NONE',  ( 0.000000000000000000, 0.000000000000000000, 1.000000000000000000 ) ) ;
#19063 = CARTESIAN_POINT ( 'NONE',  ( -82.55893756888772828, 134.8282482779731595, -15.44913056569797050 ) ) ;
#19064 = CARTESIAN_POINT ( 'NONE',  ( 157.9999999999996305, 283.6968751876750616, -45.00000000000000000 ) ) ;
#19065 = CARTESIAN_POINT ( 'NONE',  ( -12.24491960465745599, -18.01420295945611727, 100.0000000000000000 ) ) ;
#19066 = EDGE_CURVE ( 'NONE', #10216, #6088, #20249, .T. ) ;
#19067 = CARTESIAN_POINT ( 'NONE',  ( -265.0761585189258653, -165.8845232629588793, -89.57447787032170083 ) ) ;
#19068 = DIRECTION ( 'NONE',  ( 0.000000000000000000, -1.000000000000000000, 0.000000000000000000 ) ) ;
#19069 = CARTESIAN_POINT ( 'NONE',  ( 17.29390901368054045, -49.11867374189763780, 98.58151313434788676 ) ) ;
#19070 = CARTESIAN_POINT ( 'NONE',  ( -224.3725904250179610, 86.95501853435987982, -16.78161447753165092 ) ) ;
#19071 = CARTESIAN_POINT ( 'NONE',  ( 131.0301686624949014, 249.7374833449995322, -149.5158039499305573 ) ) ;
#19072 = VECTOR ( 'NONE', #26692, 1000.000000000000000 ) ;
#19073 = LINE ( 'NONE', #25674, #1169 ) ;
#19074 = CARTESIAN_POINT ( 'NONE',  ( 158.0000000000005684, 153.2873747973098659, 45.00000000000000000 ) ) ;
#19075 = DIRECTION ( 'NONE',  ( -0.000000000000000000, -0.000000000000000000, 1.000000000000000000 ) ) ;
#19076 = VECTOR ( 'NONE', #7568, 1000.000000000000000 ) ;
#19077 = CARTESIAN_POINT ( 'NONE',  ( 158.0000000000016200, 52.97237449702815582, 45.00000000000000000 ) ) ;
#19078 = AXIS2_PLACEMENT_3D ( 'NONE', #22346, #20611, #26640 ) ;
#19079 = ORIENTED_EDGE ( 'NONE', *, *, #7266, .F. ) ;
#19080 = CARTESIAN_POINT ( 'NONE',  ( -63.57415822541634043, -23.01420295945612082, 95.00000000000000000 ) ) ;
#19081 = CARTESIAN_POINT ( 'NONE',  ( 109.0192378864665557, 205.0000000000002842, -151.0000000000000284 ) ) ;
#19082 = VECTOR ( 'NONE', #26846, 1000.000000000000000 ) ;
#19084 = ORIENTED_EDGE ( 'NONE', *, *, #3536, .F. ) ;
#19083 = EDGE_LOOP ( 'NONE', ( #22740, #10323, #5056, #11426, #21335 ) ) ;
#19085 = ADVANCED_FACE ( 'NONE', ( #8553 ), #23772, .F. ) ;
#19086 = EDGE_CURVE ( 'NONE', #16305, #17073, #3660, .T. ) ;
#19087 = CARTESIAN_POINT ( 'NONE',  ( 107.9865739111623242, 251.1735473298933812, -29.61538987306452952 ) ) ;
#19088 = EDGE_CURVE ( 'NONE', #26586, #17489, #27644, .T. ) ;
#19089 = ORIENTED_EDGE ( 'NONE', *, *, #8809, .F. ) ;
#19090 = ORIENTED_EDGE ( 'NONE', *, *, #12489, .F. ) ;
#19091 = ORIENTED_EDGE ( 'NONE', *, *, #28086, .T. ) ;
#19092 = VERTEX_POINT ( 'NONE', #1374 ) ;
#19093 = ORIENTED_EDGE ( 'NONE', *, *, #2460, .T. ) ;
#19094 = ORIENTED_EDGE ( 'NONE', *, *, #23272, .F. ) ;
#19095 = VECTOR ( 'NONE', #6754, 1000.000000000000000 ) ;
#19096 = DIRECTION ( 'NONE',  ( -0.000000000000000000, 0.000000000000000000, 1.000000000000000000 ) ) ;
#19097 = FACE_BOUND ( 'NONE', #5584, .T. ) ;
#19098 = AXIS2_PLACEMENT_3D ( 'NONE', #11462, #13906, #11608 ) ;
#19099 = DIRECTION ( 'NONE',  ( 1.000000000000000000, 0.000000000000000000, 0.000000000000000000 ) ) ;
#19100 = DIRECTION ( 'NONE',  ( 0.4528218681377311206, -0.8916010070296327417, 0.000000000000000000 ) ) ;
#19101 = LINE ( 'NONE', #14656, #8475 ) ;
#19102 = ADVANCED_BREP_SHAPE_REPRESENTATION ( '', ( #28156, #10637 ), #3285 ) ;
#19103 = DIRECTION ( 'NONE',  ( 0.8916010070298867607, 0.4528218681372308541, 0.000000000000000000 ) ) ;
#19104 = CARTESIAN_POINT ( 'NONE',  ( 187.4999999999996305, 40.68693696324645970, -45.00000000000000000 ) ) ;
#19105 = LINE ( 'NONE', #25429, #407 ) ;
#19106 = CARTESIAN_POINT ( 'NONE',  ( 134.9999999999998579, 220.0000000000000284, -84.99999999999997158 ) ) ;
#19107 = CARTESIAN_POINT ( 'NONE',  ( 157.4999999999995737, 203.6988124512014338, 45.00000000000000000 ) ) ;
#19108 = DIRECTION ( 'NONE',  ( 0.8916010070293783896, -0.4528218681382319422, 0.000000000000000000 ) ) ;
#19109 = ORIENTED_EDGE ( 'NONE', *, *, #14841, .F. ) ;
#19110 = CONICAL_SURFACE ( 'NONE', #5805, 18.91107291867258411, 0.08885387018394237668 ) ;
#19111 = DIRECTION ( 'NONE',  ( -0.8516548651973804285, 0.5241030343220993704, 0.000000000000000000 ) ) ;
#19112 = EDGE_CURVE ( 'NONE', #21343, #7910, #25637, .T. ) ;
#19113 = EDGE_CURVE ( 'NONE', #10576, #2123, #6804, .T. ) ;
#19114 = DIRECTION ( 'NONE',  ( -0.000000000000000000, -0.000000000000000000, 1.000000000000000000 ) ) ;
#19115 = ORIENTED_EDGE ( 'NONE', *, *, #2323, .T. ) ;
#19116 = APPLICATION_PROTOCOL_DEFINITION ( 'draft international standard', 'automotive_design', 1998, #10020 ) ;
#19117 = VERTEX_POINT ( 'NONE', #28342 ) ;
#19118 = EDGE_LOOP ( 'NONE', ( #19339, #7780, #21390, #16553 ) ) ;
#19119 = CARTESIAN_POINT ( 'NONE',  ( 96.76194576697650973, 83.89264379418858653, 100.0000000000000142 ) ) ;
#19120 = DIRECTION ( 'NONE',  ( -0.8916010070297852863, -0.4528218681374307497, 0.000000000000000000 ) ) ;
#19121 = ORIENTED_EDGE ( 'NONE', *, *, #7556, .T. ) ;
#19122 = VERTEX_POINT ( 'NONE', #2636 ) ;
#19123 = DIRECTION ( 'NONE',  ( 0.8916010070294395629, -0.4528218681381114274, 0.000000000000000000 ) ) ;
#19124 = CARTESIAN_POINT ( 'NONE',  ( -217.0264852877946566, -91.18033988749901653, -19.68410787789781580 ) ) ;
#19125 = DIRECTION ( 'NONE',  ( -0.8916010070299577039, -0.4528218681370910215, 0.000000000000000000 ) ) ;
#19126 = EDGE_LOOP ( 'NONE', ( #24110, #18223, #4934, #10043 ) ) ;
#19127 = CARTESIAN_POINT ( 'NONE',  ( -519.6468271856125511, -175.5700023691478577, -9.184850993605147944E-16 ) ) ;
#19128 = VERTEX_POINT ( 'NONE', #13578 ) ;
#19129 = AXIS2_PLACEMENT_3D ( 'NONE', #18810, #21104, #11943 ) ;
#19130 = CARTESIAN_POINT ( 'NONE',  ( 157.9999999999996305, 284.2047501951820436, -45.00000000000000000 ) ) ;
#19131 = AXIS2_PLACEMENT_3D ( 'NONE', #12613, #25388, #19062 ) ;
#19132 = PLANE ( 'NONE',  #20393 ) ;
#19133 = CARTESIAN_POINT ( 'NONE',  ( -38.16416761298290794, 129.9976787137582335, -15.32285261404498655 ) ) ;
#19134 = DIRECTION ( 'NONE',  ( 0.8916010070296429557, 0.4528218681377111920, 0.000000000000000000 ) ) ;
#19135 = FACE_OUTER_BOUND ( 'NONE', #3537, .T. ) ;
#19136 = CARTESIAN_POINT ( 'NONE',  ( 161.1794673982064694, 205.3441676487868506, -151.0000000000000000 ) ) ;
#19137 = EDGE_CURVE ( 'NONE', #22238, #17429, #15586, .T. ) ;
#19138 = VERTEX_POINT ( 'NONE', #15449 ) ;
#19139 = DIRECTION ( 'NONE',  ( 0.000000000000000000, 0.000000000000000000, 1.000000000000000000 ) ) ;
#19140 = DIRECTION ( 'NONE',  ( -0.000000000000000000, 0.000000000000000000, 1.000000000000000000 ) ) ;
#19141 = DIRECTION ( 'NONE',  ( 0.000000000000000000, -1.000000000000000000, 0.000000000000000000 ) ) ;
#19142 = CARTESIAN_POINT ( 'NONE',  ( 157.4999999999998579, 53.22631200078164682, 45.00000000000000000 ) ) ;
#19143 = ORIENTED_EDGE ( 'NONE', *, *, #406, .T. ) ;
#19144 = CARTESIAN_POINT ( 'NONE',  ( 157.4999999999998579, 70.78143705333094715, 45.00000000000000000 ) ) ;
#19145 = ADVANCED_FACE ( 'NONE', ( #26201 ), #10989, .F. ) ;
#19146 = FACE_OUTER_BOUND ( 'NONE', #6532, .T. ) ;
#19147 = LINE ( 'NONE', #10819, #13338 ) ;
#19148 = DIRECTION ( 'NONE',  ( -0.000000000000000000, -0.000000000000000000, -1.000000000000000000 ) ) ;
#19149 = ORIENTED_EDGE ( 'NONE', *, *, #2643, .T. ) ;
#19150 =( NAMED_UNIT ( * ) PLANE_ANGLE_UNIT ( ) SI_UNIT ( $, .RADIAN. ) );
#19151 = CARTESIAN_POINT ( 'NONE',  ( 157.4999999999998579, 53.22631200078164682, 45.00000000000000000 ) ) ;
#19152 = VERTEX_POINT ( 'NONE', #24333 ) ;
#19153 = CIRCLE ( 'NONE', #15501, 33.76444293738739333 ) ;
#19154 = EDGE_CURVE ( 'NONE', #11558, #13277, #22039, .T. ) ;
#19155 = CARTESIAN_POINT ( 'NONE',  ( -213.1827219047386848, -216.7767438708612531, 95.00000000000004263 ) ) ;
#19156 = CARTESIAN_POINT ( 'NONE',  ( 158.0000000000002274, 185.8897498949014278, -45.00000000000000000 ) ) ;
#19157 = ORIENTED_EDGE ( 'NONE', *, *, #21887, .T. ) ;
#19158 = ORIENTED_EDGE ( 'NONE', *, *, #6700, .T. ) ;
#19159 = CARTESIAN_POINT ( 'NONE',  ( 157.4999999999998579, 70.78143705333094715, 45.00000000000000000 ) ) ;
#19160 = ORIENTED_EDGE ( 'NONE', *, *, #9358, .F. ) ;
#19161 = ORIENTED_EDGE ( 'NONE', *, *, #3620, .T. ) ;
#19162 = VERTEX_POINT ( 'NONE', #6527 ) ;
#19163 = EDGE_CURVE ( 'NONE', #2819, #14705, #11126, .T. ) ;
#19164 = LINE ( 'NONE', #8540, #19400 ) ;
#19165 = CIRCLE ( 'NONE', #23311, 10.71881775658151170 ) ;
#19166 = CARTESIAN_POINT ( 'NONE',  ( 158.0000000000000853, 196.4291249324366504, 45.00000000000000000 ) ) ;
#19167 = CARTESIAN_POINT ( 'NONE',  ( 0.2663009637210750902, 1.249999999999999556, 7.393443028451041954 ) ) ;
#19168 = FACE_OUTER_BOUND ( 'NONE', #1127, .T. ) ;
#19169 = CARTESIAN_POINT ( 'NONE',  ( 157.9999999999998010, 239.0630000600560550, -45.00000000000000000 ) ) ;
#19170 = EDGE_CURVE ( 'NONE', #7680, #6925, #20022, .T. ) ;
#19171 = CARTESIAN_POINT ( 'NONE',  ( -225.5243807178691782, 62.25611586198358793, -19.08347035850416518 ) ) ;
#19172 = ORIENTED_EDGE ( 'NONE', *, *, #4838, .F. ) ;
#19173 = CARTESIAN_POINT ( 'NONE',  ( 33.10302365956999182, 203.2034914284457159, 12.99999999999999822 ) ) ;
#19174 = DIRECTION ( 'NONE',  ( -0.8916010070293595158, -0.4528218681382693567, 0.000000000000000000 ) ) ;
#19175 = DIRECTION ( 'NONE',  ( -0.000000000000000000, -0.000000000000000000, -1.000000000000000000 ) ) ;
#19176 = DIRECTION ( 'NONE',  ( -0.000000000000000000, -0.000000000000000000, -1.000000000000000000 ) ) ;
#19177 = ORIENTED_EDGE ( 'NONE', *, *, #10039, .F. ) ;
#19178 = CARTESIAN_POINT ( 'NONE',  ( 157.9999999999996589, 281.1890001801680796, 45.00000000000000000 ) ) ;
#19179=STYLED_ITEM('',(#28420),#27918);
#19180 = CARTESIAN_POINT ( 'NONE',  ( 158.0000000000001137, 193.9212499249295831, -45.00000000000000000 ) ) ;
#19181 = DIRECTION ( 'NONE',  ( 1.000000000000000000, -8.326672684688676025E-16, 0.000000000000000000 ) ) ;
#19182 = PLANE ( 'NONE',  #19473 ) ;
#19183 = DIRECTION ( 'NONE',  ( 0.000000000000000000, 1.000000000000000000, -0.000000000000000000 ) ) ;
#19184 = LINE ( 'NONE', #27931, #5142 ) ;
#19185 = ORIENTED_EDGE ( 'NONE', *, *, #17328, .T. ) ;
#19186 = AXIS2_PLACEMENT_3D ( 'NONE', #24521, #11165, #20058 ) ;
#19187 = EDGE_CURVE ( 'NONE', #7590, #1943, #11279, .T. ) ;
#19188 = FACE_OUTER_BOUND ( 'NONE', #16031, .T. ) ;
#19189 = ORIENTED_EDGE ( 'NONE', *, *, #4414, .T. ) ;
#19190 = EDGE_CURVE ( 'NONE', #2326, #27871, #22183, .T. ) ;
#19191 = DIRECTION ( 'NONE',  ( 0.4528218681382912836, -0.8916010070293483025, 0.000000000000000000 ) ) ;
#19192 = CIRCLE ( 'NONE', #7720, 100.0000000000000284 ) ;
#19193 = EDGE_LOOP ( 'NONE', ( #19234, #25546, #22759, #11362 ) ) ;
#19194 = ORIENTED_EDGE ( 'NONE', *, *, #27785, .F. ) ;
#19195 = CARTESIAN_POINT ( 'NONE',  ( 158.0000000000015348, 60.49599951954928656, 45.00000000000000000 ) ) ;
#19196 = ORIENTED_EDGE ( 'NONE', *, *, #3155, .T. ) ;
#19197 = ORIENTED_EDGE ( 'NONE', *, *, #2599, .T. ) ;
#19198 = CARTESIAN_POINT ( 'NONE',  ( 113.5875366493125682, 213.0176248557028487, 97.68174538100568327 ) ) ;
#19199 = EDGE_CURVE ( 'NONE', #16733, #9066, #353, .T. ) ;
#19200 = DIRECTION ( 'NONE',  ( -0.000000000000000000, -0.000000000000000000, -1.000000000000000000 ) ) ;
#19201 = LINE ( 'NONE', #10872, #24906 ) ;
#19202 = AXIS2_PLACEMENT_3D ( 'NONE', #27020, #5041, #9075 ) ;
#19203 = DIRECTION ( 'NONE',  ( -0.000000000000000000, 0.000000000000000000, -1.000000000000000000 ) ) ;
#19204 = EDGE_CURVE ( 'NONE', #8066, #18076, #21763, .T. ) ;
#19205 = CARTESIAN_POINT ( 'NONE',  ( 158.0000000000005116, 160.8109998198309825, 45.00000000000000000 ) ) ;
#19207 = PLANE ( 'NONE',  #395 ) ;
#19206 = VECTOR ( 'NONE', #498, 1000.000000000000000 ) ;
#19208 = CARTESIAN_POINT ( 'NONE',  ( 25.98252322492246691, -45.47589623052219565, 99.52282825389700349 ) ) ;
#19209 = CARTESIAN_POINT ( 'NONE',  ( -227.1071502729981830, 87.87580414022654907, -15.87121314882625889 ) ) ;
#19210 = PRODUCT ( 'Gear Rack', 'Gear Rack', '', ( #26145 ) ) ;
#19211 = FACE_OUTER_BOUND ( 'NONE', #16137, .T. ) ;
#19212 = AXIS2_PLACEMENT_3D ( 'NONE', #5290, #27530, #5713 ) ;
#19213 = DIRECTION ( 'NONE',  ( 0.000000000000000000, -1.000000000000000000, 0.000000000000000000 ) ) ;
#19214 = EDGE_CURVE ( 'NONE', #25157, #15447, #26623, .T. ) ;
#19215 = LINE ( 'NONE', #8447, #1881 ) ;
#19216 = CARTESIAN_POINT ( 'NONE',  ( 217.4999999999996305, 0.000000000000000000, 0.000000000000000000 ) ) ;
#19217 = CYLINDRICAL_SURFACE ( 'NONE', #3822, 30.00000000000000000 ) ;
#19218 = ORIENTED_EDGE ( 'NONE', *, *, #27847, .T. ) ;
#19219 = VECTOR ( 'NONE', #17255, 1000.000000000000000 ) ;
#19220 = DIRECTION ( 'NONE',  ( 0.000000000000000000, -1.000000000000000000, 0.000000000000000000 ) ) ;
#19221 = CARTESIAN_POINT ( 'NONE',  ( 167.4999999999996589, 258.6181251126050711, -5.999999999999991118 ) ) ;
#19222 = CARTESIAN_POINT ( 'NONE',  ( 158.0000000000005969, 148.7794997898028271, 45.00000000000000000 ) ) ;
#19224 = VERTEX_POINT ( 'NONE', #2204 ) ;
#19223 = VERTEX_POINT ( 'NONE', #13018 ) ;
#19225 = CIRCLE ( 'NONE', #13750, 72.21503689626329958 ) ;
#19226 = CARTESIAN_POINT ( 'NONE',  ( 91.66503723320899155, 240.0531355366297817, -6.981029948440879984 ) ) ;
#19227 = ORIENTED_EDGE ( 'NONE', *, *, #21711, .F. ) ;
#19228 = VERTEX_POINT ( 'NONE', #17442 ) ;
#19229 = AXIS2_PLACEMENT_3D ( 'NONE', #4417, #22089, #19933 ) ;
#19230 = ORIENTED_EDGE ( 'NONE', *, *, #17888, .F. ) ;
#19231 = AXIS2_PLACEMENT_3D ( 'NONE', #7743, #3846, #12490 ) ;
#19232 = ORIENTED_EDGE ( 'NONE', *, *, #16661, .F. ) ;
#19233 = ORIENTED_EDGE ( 'NONE', *, *, #313, .T. ) ;
#19234 = ORIENTED_EDGE ( 'NONE', *, *, #11548, .F. ) ;
#19235 = DIRECTION ( 'NONE',  ( -0.8916010070293409751, -0.4528218681383056610, 0.000000000000000000 ) ) ;
#19236 = AXIS2_PLACEMENT_3D ( 'NONE', #7488, #18812, #11670 ) ;
#19237 = CARTESIAN_POINT ( 'NONE',  ( -412.2374841615667833, -120.0000000000002558, 100.0000000000000142 ) ) ;
#19238 = EDGE_CURVE ( 'NONE', #2342, #22383, #18893, .T. ) ;
#19239 = DIRECTION ( 'NONE',  ( 0.000000000000000000, 0.000000000000000000, -1.000000000000000000 ) ) ;
#19240 = ADVANCED_FACE ( 'NONE', ( #24197 ), #19739, .F. ) ;
#19241 = CARTESIAN_POINT ( 'NONE',  ( -17.24491960465747553, 24.64876300893806160, 100.0000000000000000 ) ) ;
#19242 = VECTOR ( 'NONE', #579, 1000.000000000000000 ) ;
#19243 = VECTOR ( 'NONE', #12458, 1000.000000000000000 ) ;
#19244 = LINE ( 'NONE', #21254, #27728 ) ;
#19245 = LINE ( 'NONE', #16535, #28375 ) ;
#19246 = CARTESIAN_POINT ( 'NONE',  ( -231.4535743690441905, 76.02244276923478594, -15.77072033396453499 ) ) ;
#19247 = AXIS2_PLACEMENT_3D ( 'NONE', #21770, #23641, #2077 ) ;
#19248 = CARTESIAN_POINT ( 'NONE',  ( -43.02437977270766112, 129.7200458115293031, 16.81627168235288039 ) ) ;
#19249 = CARTESIAN_POINT ( 'NONE',  ( 124.9999999999998579, 220.0000000000000284, -119.9999999999999858 ) ) ;
#19250 = DIRECTION ( 'NONE',  ( 1.000000000000000000, 0.000000000000000000, 0.000000000000000000 ) ) ;
#19251 = DIRECTION ( 'NONE',  ( 1.000000000000000000, 0.000000000000000000, 0.000000000000000000 ) ) ;
#19252 = ORIENTED_EDGE ( 'NONE', *, *, #15652, .F. ) ;
#19253 = CARTESIAN_POINT ( 'NONE',  ( -200.1276905507725985, 95.64193732372173429, 30.67736252160736399 ) ) ;
#19254 = AXIS2_PLACEMENT_3D ( 'NONE', #12336, #8293, #17752 ) ;
#19255 = PLANE ( 'NONE',  #8969 ) ;
#19256 = VERTEX_POINT ( 'NONE', #10846 ) ;
#19257 = APPLICATION_PROTOCOL_DEFINITION ( 'draft international standard', 'automotive_design', 1998, #8003 ) ;
#19258 = ORIENTED_EDGE ( 'NONE', *, *, #20375, .T. ) ;
#19259 = ORIENTED_EDGE ( 'NONE', *, *, #25914, .T. ) ;
#19260 = CARTESIAN_POINT ( 'NONE',  ( 109.6721745451680334, 96.60743919220468001, 100.0000000000000142 ) ) ;
#19261 = EDGE_CURVE ( 'NONE', #26578, #855, #24483, .T. ) ;
#19262 = CARTESIAN_POINT ( 'NONE',  ( 157.9999999999996589, 274.1732501651540588, -45.00000000000000000 ) ) ;
#19263 = B_SPLINE_CURVE_WITH_KNOTS ( 'NONE', 3,
 ( #25370, #14321, #14599, #19044, #18902, #3525, #27369, #7844, #5692, #21056, #20773, #12598, #16478, #12176, #1381, #14462, #10006, #7576, #21337, #7988, #10288, #1657, #22937, #12314, #14184, #20917, #1097, #23219 ),
 .UNSPECIFIED., .F., .F.,
 ( 4, 2, 2, 2, 2, 2, 2, 2, 2, 2, 2, 2, 2, 4 ),
 ( -4.016943939060031455E-05, 0.006308104419754258403, 0.01265637827889911672, 0.01900465213804397591, 0.02217878906761640637, 0.02535292599718883336, 0.03170119985633366305, 0.03487533678590611086, 0.03804947371547856561, 0.04122361064505101341, 0.04281067910983723385, 0.04439774757462346122, 0.04757188450419585352, 0.05074602143376824581 ),
 .UNSPECIFIED. ) ;
#19264 = ORIENTED_EDGE ( 'NONE', *, *, #19789, .F. ) ;
#19265 = VERTEX_POINT ( 'NONE', #63 ) ;
#19266 = CARTESIAN_POINT ( 'NONE',  ( 108.2273028577067322, 129.5338070840588216, -100.0000000000000142 ) ) ;
#19267 = VECTOR ( 'NONE', #14292, 1000.000000000000114 ) ;
#19268 = DIRECTION ( 'NONE',  ( -0.000000000000000000, 1.000000000000000000, -1.387778780781445429E-16 ) ) ;
#19269 = LINE ( 'NONE', #15258, #4997 ) ;
#19270 = ORIENTED_EDGE ( 'NONE', *, *, #23888, .T. ) ;
#19271 = EDGE_CURVE ( 'NONE', #22091, #20823, #9264, .T. ) ;
#19272 = CARTESIAN_POINT ( 'NONE',  ( -230.9997220956770150, 90.08100258884712730, 15.10258885251132455 ) ) ;
#19273 = VERTEX_POINT ( 'NONE', #26780 ) ;
#19274 = DIRECTION ( 'NONE',  ( -0.000000000000000000, 1.000000000000000000, -1.387778780781445429E-16 ) ) ;
#19275 = EDGE_CURVE ( 'NONE', #968, #9708, #21642, .T. ) ;
#19276 = EDGE_CURVE ( 'NONE', #17217, #17245, #19481, .T. ) ;
#19277 = ADVANCED_FACE ( 'NONE', ( #26921 ), #9686, .F. ) ;
#19278 = CARTESIAN_POINT ( 'NONE',  ( -175.0000000000000000, -170.0000000000001990, -69.99999999999998579 ) ) ;
#19279 = DIRECTION ( 'NONE',  ( -1.000000000000000000, 0.000000000000000000, 0.000000000000000000 ) ) ;
#19280 = FACE_OUTER_BOUND ( 'NONE', #1418, .T. ) ;
#19281 = ORIENTED_EDGE ( 'NONE', *, *, #28365, .F. ) ;
#19282 = VECTOR ( 'NONE', #7977, 999.9999999999998863 ) ;
#19283 = DIRECTION ( 'NONE',  ( 0.000000000000000000, -1.000000000000000000, 0.000000000000000000 ) ) ;
#19284 = FACE_BOUND ( 'NONE', #25309, .T. ) ;
#19285 = PLANE ( 'NONE',  #19811 ) ;
#19286 = DIRECTION ( 'NONE',  ( -0.000000000000000000, -0.000000000000000000, -1.000000000000000000 ) ) ;
#19287 = ORIENTED_EDGE ( 'NONE', *, *, #7211, .T. ) ;
#19288 = CARTESIAN_POINT ( 'NONE',  ( -119.0030847931093518, 214.2064521616283059, -15.00000000000000000 ) ) ;
#19289 = AXIS2_PLACEMENT_3D ( 'NONE', #8655, #23882, #4332 ) ;
#19290 = LINE ( 'NONE', #19432, #13006 ) ;
#19291 = DIRECTION ( 'NONE',  ( -6.938893903907227392E-16, -1.000000000000000000, 0.000000000000000000 ) ) ;
#19292 = DIRECTION ( 'NONE',  ( 0.000000000000000000, 0.000000000000000000, 1.000000000000000000 ) ) ;
#19293 = ORIENTED_EDGE ( 'NONE', *, *, #14878, .F. ) ;
#19294 = DIRECTION ( 'NONE',  ( 1.000000000000000000, 0.000000000000000000, 0.000000000000000000 ) ) ;
#19295 = ORIENTED_EDGE ( 'NONE', *, *, #17521, .T. ) ;
#19296 = CYLINDRICAL_SURFACE ( 'NONE', #11584, 5.999999999999991118 ) ;
#19297 = CARTESIAN_POINT ( 'NONE',  ( -178.6577177197984270, 110.8366912208841200, -29.80435504473049591 ) ) ;
#19298 = EDGE_LOOP ( 'NONE', ( #8450, #18871, #4919, #24795 ) ) ;
#19299 = ORIENTED_EDGE ( 'NONE', *, *, #11374, .F. ) ;
#19300 = LINE ( 'NONE', #16454, #16821 ) ;
#19301 = ADVANCED_FACE ( 'NONE', ( #20594 ), #23034, .T. ) ;
#19302 = VERTEX_POINT ( 'NONE', #643 ) ;
#19303 = ADVANCED_FACE ( 'NONE', ( #16019 ), #11990, .F. ) ;
#19304 = AXIS2_PLACEMENT_3D ( 'NONE', #984, #16507, #20809 ) ;
#19305 = EDGE_CURVE ( 'NONE', #12668, #7560, #27331, .T. ) ;
#19306 = EDGE_LOOP ( 'NONE', ( #14394, #5868, #27976 ) ) ;
#19307 = VERTEX_POINT ( 'NONE', #3344 ) ;
#19308 = PLANE ( 'NONE',  #20778 ) ;
#19309 = VECTOR ( 'NONE', #609, 1000.000000000000114 ) ;
#19310 = EDGE_CURVE ( 'NONE', #25194, #477, #11714, .T. ) ;
#19311 = DIRECTION ( 'NONE',  ( -0.000000000000000000, 0.000000000000000000, 1.000000000000000000 ) ) ;
#19312 = CARTESIAN_POINT ( 'NONE',  ( 122.8247714198256944, 204.1329331941749672, -45.00000000000000000 ) ) ;
#19313 = PLANE ( 'NONE',  #27762 ) ;
#19314 = LINE ( 'NONE', #10138, #3690 ) ;
#19315 = FACE_OUTER_BOUND ( 'NONE', #13177, .T. ) ;
#19316 = ORIENTED_EDGE ( 'NONE', *, *, #27628, .T. ) ;
#19317 = LINE ( 'NONE', #3518, #17721 ) ;
#19318 = DIRECTION ( 'NONE',  ( -0.8916010070293584056, 0.4528218681382713551, 0.000000000000000000 ) ) ;
#19319 = DIRECTION ( 'NONE',  ( 1.000000000000000000, 0.000000000000000000, 0.000000000000000000 ) ) ;
#19320 = LINE ( 'NONE', #25924, #25860 ) ;
#19321 = ORIENTED_EDGE ( 'NONE', *, *, #20957, .F. ) ;
#19322 = DIRECTION ( 'NONE',  ( -0.5457381880580733924, -0.8379557447115515423, 0.000000000000000000 ) ) ;
#19323 = VECTOR ( 'NONE', #27957, 1000.000000000000000 ) ;
#19324 = DIRECTION ( 'NONE',  ( 0.8660254037844432595, 0.4999999999999919509, -0.000000000000000000 ) ) ;
#19325 = CARTESIAN_POINT ( 'NONE',  ( -268.1539709403929805, -165.4081636382954343, 88.87781807846162963 ) ) ;
#19326 = FACE_OUTER_BOUND ( 'NONE', #3455, .T. ) ;
#19327 = DIRECTION ( 'NONE',  ( 4.540956701092242152E-16, 1.000000000000000000, 0.000000000000000000 ) ) ;
#19328 = CARTESIAN_POINT ( 'NONE',  ( 157.4999999999997726, 248.8405625863305204, 45.00000000000000000 ) ) ;
#19329 = VERTEX_POINT ( 'NONE', #2929 ) ;
#19330 = AXIS2_PLACEMENT_3D ( 'NONE', #16346, #11760, #20776 ) ;
#19331 = CYLINDRICAL_SURFACE ( 'NONE', #11156, 22.49999999999999289 ) ;
#19332 = ORIENTED_EDGE ( 'NONE', *, *, #4030, .F. ) ;
#19333 = LINE ( 'NONE', #25936, #19527 ) ;
#19334 = ORIENTED_EDGE ( 'NONE', *, *, #24812, .F. ) ;
#19335 = VERTEX_POINT ( 'NONE', #16158 ) ;
#19336 = DIRECTION ( 'NONE',  ( -0.000000000000000000, 0.000000000000000000, -1.000000000000000000 ) ) ;
#19337 = EDGE_CURVE ( 'NONE', #8321, #18107, #18446, .T. ) ;
#19338 = ORIENTED_EDGE ( 'NONE', *, *, #7121, .F. ) ;
#19339 = ORIENTED_EDGE ( 'NONE', *, *, #22325, .T. ) ;
#19340 = DIRECTION ( 'NONE',  ( 0.000000000000000000, 0.000000000000000000, -1.000000000000000000 ) ) ;
#19341 = CARTESIAN_POINT ( 'NONE',  ( -122.3728877774221644, 131.4092382197305255, -16.24378286920686421 ) ) ;
#19342 = DIRECTION ( 'NONE',  ( 0.000000000000000000, -1.000000000000000000, -0.000000000000000000 ) ) ;
#19343 = CARTESIAN_POINT ( 'NONE',  ( -144.5013834658754206, 126.7803687903472820, -18.02807566880128931 ) ) ;
#19344 = VECTOR ( 'NONE', #20142, 1000.000000000000000 ) ;
#19345 = VECTOR ( 'NONE', #19471, 1000.000000000000000 ) ;
#19346 = VECTOR ( 'NONE', #2970, 1000.000000000000000 ) ;
#19347 = CARTESIAN_POINT ( 'NONE',  ( -265.2785062999343495, -171.0615922813920804, -89.54987397248345360 ) ) ;
#19348 = CARTESIAN_POINT ( 'NONE',  ( -270.7452880837828388, -170.3087097900280753, 93.46977427553774476 ) ) ;
#19349 = CARTESIAN_POINT ( 'NONE',  ( -225.8617995309101047, 89.52870790985693361, -13.92929402531509098 ) ) ;
#19350 = EDGE_CURVE ( 'NONE', #8779, #28324, #5365, .T. ) ;
#19351 = EDGE_CURVE ( 'NONE', #17645, #18325, #2832, .T. ) ;
#19352 = CARTESIAN_POINT ( 'NONE',  ( 131.3319829069345417, 249.7767514970616674, -149.7646631383025237 ) ) ;
#19353 = CARTESIAN_POINT ( 'NONE',  ( -229.0059842468561442, 88.86886271388162584, 15.45135540806963448 ) ) ;
#19354 = FACE_OUTER_BOUND ( 'NONE', #1361, .T. ) ;
#19355 = FACE_OUTER_BOUND ( 'NONE', #25692, .T. ) ;
#19356 = CARTESIAN_POINT ( 'NONE',  ( 157.4999999999998579, 166.0806873385985796, 45.00000000000000000 ) ) ;
#19357 = ORIENTED_EDGE ( 'NONE', *, *, #21902, .T. ) ;
#19358 = FACE_OUTER_BOUND ( 'NONE', #13886, .T. ) ;
#19359 = LINE ( 'NONE', #6431, #28187 ) ;
#19360 = DIRECTION ( 'NONE',  ( 0.000000000000000000, 1.000000000000000000, -1.224646799147353207E-16 ) ) ;
#19362 = EDGE_LOOP ( 'NONE', ( #10802, #3826, #8283, #4364 ) ) ;
#19361 = ORIENTED_EDGE ( 'NONE', *, *, #12521, .F. ) ;
#19363 = ADVANCED_FACE ( 'NONE', ( #7536 ), #24773, .F. ) ;
#19364 = EDGE_CURVE ( 'NONE', #25296, #2640, #14011, .T. ) ;
#19365 = VECTOR ( 'NONE', #16957, 1000.000000000000000 ) ;
#19366 = CARTESIAN_POINT ( 'NONE',  ( 105.1668099567758077, 241.3986356328212821, -28.65150506302982336 ) ) ;
#19367 = ORIENTED_EDGE ( 'NONE', *, *, #27028, .F. ) ;
#19368 = B_SPLINE_CURVE_WITH_KNOTS ( 'NONE', 3,
 ( #27809, #4255, #8147, #25806, #6132, #13042, #23801, #10735, #6414, #15191, #28364, #23943, #21789, #2096, #8714, #17468 ),
 .UNSPECIFIED., .F., .F.,
 ( 4, 2, 2, 2, 2, 2, 2, 4 ),
 ( 0.000000000000000000, 0.001557302553632627148, 0.002335953830448963056, 0.003114605107265298531, 0.004671907660897984226, 0.005450558937714350925, 0.005839884576122509122, 0.006229210214530666451 ),
 .UNSPECIFIED. ) ;
#19369 = ORIENTED_EDGE ( 'NONE', *, *, #13285, .F. ) ;
#19370 = AXIS2_PLACEMENT_3D ( 'NONE', #2438, #19690, #15106 ) ;
#19371 =( GEOMETRIC_REPRESENTATION_CONTEXT ( 3 ) GLOBAL_UNCERTAINTY_ASSIGNED_CONTEXT ( ( #26402 ) ) GLOBAL_UNIT_ASSIGNED_CONTEXT ( ( #26034, #24037, #13131 ) ) REPRESENTATION_CONTEXT ( 'NONE', 'WORKASPACE' ) );
#19372 = VERTEX_POINT ( 'NONE', #16300 ) ;
#19373 = VECTOR ( 'NONE', #21199, 1000.000000000000000 ) ;
#19374 = ORIENTED_EDGE ( 'NONE', *, *, #20746, .F. ) ;
#19375 = ORIENTED_EDGE ( 'NONE', *, *, #7432, .T. ) ;
#19376 = ORIENTED_EDGE ( 'NONE', *, *, #3300, .F. ) ;
#19377 = LINE ( 'NONE', #26264, #22379 ) ;
#19378 = CARTESIAN_POINT ( 'NONE',  ( 217.4999999999996305, 83.06687458711267880, 42.86484227207692754 ) ) ;
#19379 = DIRECTION ( 'NONE',  ( 1.000000000000000000, -0.000000000000000000, -0.000000000000000000 ) ) ;
#19380 = VECTOR ( 'NONE', #27668, 1000.000000000000114 ) ;
#19381 = DIRECTION ( 'NONE',  ( 0.000000000000000000, -1.000000000000000000, 0.000000000000000000 ) ) ;
#19382 = EDGE_CURVE ( 'NONE', #5381, #16287, #3062, .T. ) ;
#19383 = VECTOR ( 'NONE', #7181, 1000.000000000000000 ) ;
#19384 = DIRECTION ( 'NONE',  ( 1.000000000000000000, 1.321694076934710155E-16, 0.000000000000000000 ) ) ;
#19385 = AXIS2_PLACEMENT_3D ( 'NONE', #28275, #8619, #21399 ) ;
#19386 = CARTESIAN_POINT ( 'NONE',  ( -214.3828916364065833, 175.2783111443768576, -15.00000000000000000 ) ) ;
#19387 = CARTESIAN_POINT ( 'NONE',  ( 153.4775906502255509, 227.6536686473015436, 45.00000000000000000 ) ) ;
#19388 = VECTOR ( 'NONE', #10258, 1000.000000000000000 ) ;
#19389 = CARTESIAN_POINT ( 'NONE',  ( 232.4999999999996305, 133.0668745871126930, 30.86484227207697018 ) ) ;
#19390 = CARTESIAN_POINT ( 'NONE',  ( 157.9999999999998295, 228.5236250225210313, 45.00000000000000000 ) ) ;
#19391 = DIRECTION ( 'NONE',  ( -1.000000000000000000, 0.000000000000000000, -0.000000000000000000 ) ) ;
#19392 = CARTESIAN_POINT ( 'NONE',  ( 158.0000000000013074, 81.06687458711267880, 45.00000000000000000 ) ) ;
#19393 = ORIENTED_EDGE ( 'NONE', *, *, #28365, .T. ) ;
#19394 = CARTESIAN_POINT ( 'NONE',  ( -184.3146016691900684, 107.2832362814925773, 31.16566266176597821 ) ) ;
#19395 = CARTESIAN_POINT ( 'NONE',  ( 134.9999999999998579, 220.0000000000000284, 90.00000000000002842 ) ) ;
#19396 = ORIENTED_EDGE ( 'NONE', *, *, #23138, .T. ) ;
#19397 = SHAPE_DEFINITION_REPRESENTATION ( #8194, #24038 ) ;
#19398 = VERTEX_POINT ( 'NONE', #9547 ) ;
#19399 = EDGE_CURVE ( 'NONE', #26105, #6540, #7392, .T. ) ;
#19400 = VECTOR ( 'NONE', #23906, 1000.000000000000000 ) ;
#19402 = ADVANCED_FACE ( 'NONE', ( #18721 ), #7100, .F. ) ;
#19401 = VERTEX_POINT ( 'NONE', #14284 ) ;
#19403 = VECTOR ( 'NONE', #13731, 1000.000000000000000 ) ;
#19404 = DIRECTION ( 'NONE',  ( -0.000000000000000000, -0.000000000000000000, -1.000000000000000000 ) ) ;
#19405 = CARTESIAN_POINT ( 'NONE',  ( -254.4816742664885965, 103.7585653882801182, 15.00000000000000000 ) ) ;
#19406 = ORIENTED_EDGE ( 'NONE', *, *, #10014, .F. ) ;
#19407 = EDGE_CURVE ( 'NONE', #17314, #12327, #16715, .T. ) ;
#19408 = VECTOR ( 'NONE', #28103, 1000.000000000000000 ) ;
#19409 = VERTEX_POINT ( 'NONE', #1336 ) ;
#19410 = CARTESIAN_POINT ( 'NONE',  ( 99.60675733924797726, 85.63108538499818678, -100.0000000000000284 ) ) ;
#19411 = CIRCLE ( 'NONE', #10701, 5.000000000000004441 ) ;
#19412 = CARTESIAN_POINT ( 'NONE',  ( 179.9999999999999147, 0.000000000000000000, -84.99999999999997158 ) ) ;
#19413 = PLANE ( 'NONE',  #24744 ) ;
#19414 = ORIENTED_EDGE ( 'NONE', *, *, #22913, .F. ) ;
#19415 = CARTESIAN_POINT ( 'NONE',  ( -212.5733778118419082, 87.16562594403421826, 23.37021847070533553 ) ) ;
#19416 = ORIENTED_EDGE ( 'NONE', *, *, #11827, .T. ) ;
#19417 = CARTESIAN_POINT ( 'NONE',  ( -295.0000000000001705, -165.0000000000001137, -110.0000000000000426 ) ) ;
#19418 = B_SPLINE_CURVE_WITH_KNOTS ( 'NONE', 3,
 ( #10025, #18781, #20795, #18642, #27387, #11913, #973, #25527, #7593, #7861, #5847, #7728, #16494 ),
 .UNSPECIFIED., .F., .F.,
 ( 4, 2, 2, 1, 2, 2, 4 ),
 ( 0.000000000000000000, 0.001215484442346315792, 0.001823226663519458618, 0.002430968884692601226, 0.003038711105865744052, 0.003646453327038886878, 0.004861937769385192044 ),
 .UNSPECIFIED. ) ;
#19419 = CARTESIAN_POINT ( 'NONE',  ( -175.0000000000000000, -120.0000000000001847, -75.99999999999998579 ) ) ;
#19420 = CARTESIAN_POINT ( 'NONE',  ( 159.6524665415090283, 202.9035392909954965, -139.5328759577091375 ) ) ;
#19421 = AXIS2_PLACEMENT_3D ( 'NONE', #3576, #27840, #4003 ) ;
#19422 = CARTESIAN_POINT ( 'NONE',  ( -244.5479615644635771, 75.99513337129096158, -5.000000000000004441 ) ) ;
#19423 = VERTEX_POINT ( 'NONE', #16575 ) ;
#19424 = CIRCLE ( 'NONE', #3341, 30.00000000000000000 ) ;
#19425 = DIRECTION ( 'NONE',  ( -1.000000000000000000, 0.000000000000000000, 0.000000000000000000 ) ) ;
#19426 = DIRECTION ( 'NONE',  ( -0.000000000000000000, -0.000000000000000000, -1.000000000000000000 ) ) ;
#19427 = CARTESIAN_POINT ( 'NONE',  ( 79.99999999999994316, -100.0000000000000284, 70.00000000000001421 ) ) ;
#19428 = VECTOR ( 'NONE', #13725, 1000.000000000000000 ) ;
#19429 = CARTESIAN_POINT ( 'NONE',  ( 158.0000000000010232, 106.1456246621830957, 45.00000000000000000 ) ) ;
#19430 = VERTEX_POINT ( 'NONE', #7808 ) ;
#19431 = CARTESIAN_POINT ( 'NONE',  ( 184.9999999999999432, -327.2004514666934369, 84.99999999999995737 ) ) ;
#19432 = CARTESIAN_POINT ( 'NONE',  ( 157.4999999999996589, 273.9193126614005678, 45.00000000000000000 ) ) ;
#19433 = CARTESIAN_POINT ( 'NONE',  ( 372.9108539694884144, -5.589247009368149222, 1.243177022048955014E-14 ) ) ;
#19434 = LINE ( 'NONE', #15282, #9880 ) ;
#19435 = ORIENTED_EDGE ( 'NONE', *, *, #22707, .F. ) ;
#19436 = CARTESIAN_POINT ( 'NONE',  ( -146.6428522700808230, 17.24192588826928585, 83.00000000000001421 ) ) ;
#19437 = EDGE_CURVE ( 'NONE', #1905, #7826, #12415, .T. ) ;
#19438 = ORIENTED_EDGE ( 'NONE', *, *, #12644, .T. ) ;
#19439 = ADVANCED_FACE ( 'NONE', ( #25467 ), #12274, .F. ) ;
#19440 = CARTESIAN_POINT ( 'NONE',  ( 179.9999999999999147, 0.000000000000000000, -100.0000000000000142 ) ) ;
#19441 = ADVANCED_FACE ( 'NONE', ( #5789 ), #12698, .F. ) ;
#19442 = CARTESIAN_POINT ( 'NONE',  ( -183.8717786033620882, 107.3112658120104470, -31.96029808677420547 ) ) ;
#19443 = ORIENTED_EDGE ( 'NONE', *, *, #21543, .T. ) ;
#19444 = VECTOR ( 'NONE', #21826, 1000.000000000000000 ) ;
#19445 = ORIENTED_EDGE ( 'NONE', *, *, #1018, .F. ) ;
#19446 = LINE ( 'NONE', #8952, #17739 ) ;
#19447 = ORIENTED_EDGE ( 'NONE', *, *, #20319, .T. ) ;
#19448 = PRODUCT_DEFINITION_SHAPE ( 'NONE', 'NONE',  #28404 ) ;
#19449 = ORIENTED_EDGE ( 'NONE', *, *, #17687, .T. ) ;
#19450 = ORIENTED_EDGE ( 'NONE', *, *, #7641, .F. ) ;
#19451 = VECTOR ( 'NONE', #15209, 1000.000000000000000 ) ;
#19452 = LINE ( 'NONE', #8398, #12549 ) ;
#19453 = LINE ( 'NONE', #28195, #16323 ) ;
#19454 = DIRECTION ( 'NONE',  ( 1.000000000000000000, 0.000000000000000000, -0.000000000000000000 ) ) ;
#19455 = CARTESIAN_POINT ( 'NONE',  ( 89.99999999999988631, 230.0000000000000000, 6.270166537925822681 ) ) ;
#19456 = DIRECTION ( 'NONE',  ( 0.8916010070295719014, 0.4528218681378510801, 0.000000000000000000 ) ) ;
#19457 = CARTESIAN_POINT ( 'NONE',  ( 158.0000000000014211, 68.52749954957745615, 45.00000000000000000 ) ) ;
#19458 = CARTESIAN_POINT ( 'NONE',  ( -243.5753208290373948, 74.80993601159312334, -14.84129168368860796 ) ) ;
#19459 = VERTEX_POINT ( 'NONE', #18860 ) ;
#19460 = DIRECTION ( 'NONE',  ( 0.000000000000000000, -1.000000000000000000, 0.000000000000000000 ) ) ;
#19461 = CARTESIAN_POINT ( 'NONE',  ( 206.2214737538543829, 104.7347325308398354, 45.00000000000000000 ) ) ;
#19462 = CARTESIAN_POINT ( 'NONE',  ( 147.3660254037845334, 200.5814157129577779, -45.00000000000000000 ) ) ;
#19463 = LINE ( 'NONE', #3809, #9820 ) ;
#19464 = ORIENTED_EDGE ( 'NONE', *, *, #9256, .T. ) ;
#19465 = VECTOR ( 'NONE', #14003, 1000.000000000000000 ) ;
#19466 = FACE_OUTER_BOUND ( 'NONE', #17005, .T. ) ;
#19467 = ADVANCED_FACE ( 'NONE', ( #27608 ), #25327, .F. ) ;
#19468 = LINE ( 'NONE', #18659, #131 ) ;
#19469 = CARTESIAN_POINT ( 'NONE',  ( 157.4999999999994600, 213.7303124812313513, -45.00000000000000000 ) ) ;
#19470 = PLANE ( 'NONE',  #12168 ) ;
#19471 = DIRECTION ( 'NONE',  ( -0.000000000000000000, -1.000000000000000000, -0.000000000000000000 ) ) ;
#19472 = LINE ( 'NONE', #8276, #25784 ) ;
#19473 = AXIS2_PLACEMENT_3D ( 'NONE', #6537, #25929, #2078 ) ;
#19474 = ORIENTED_EDGE ( 'NONE', *, *, #678, .F. ) ;
#19475 = ADVANCED_FACE ( 'NONE', ( #10528 ), #19285, .F. ) ;
#19476 = FACE_OUTER_BOUND ( 'NONE', #27830, .T. ) ;
#19477 = ORIENTED_EDGE ( 'NONE', *, *, #16431, .F. ) ;
#19478 = ADVANCED_FACE ( 'NONE', ( #3623 ), #25888, .F. ) ;
#19479 = DIRECTION ( 'NONE',  ( 0.4999999999999920064, -0.8660254037844432595, 0.000000000000000000 ) ) ;
#19480 = ORIENTED_EDGE ( 'NONE', *, *, #26431, .F. ) ;
#19481 = B_SPLINE_CURVE_WITH_KNOTS ( 'NONE', 3,
 ( #13868, #25185, #27058, #1058, #24627, #18169, #11851, #12136, #18307 ),
 .UNSPECIFIED., .F., .F.,
 ( 4, 2, 1, 2, 4 ),
 ( 0.000000000000000000, 0.003993085574633965795, 0.007986171149267931590, 0.01197925672390189739, 0.01597234229853586318 ),
 .UNSPECIFIED. ) ;
#19482 = ORIENTED_EDGE ( 'NONE', *, *, #10406, .T. ) ;
#19483 = FACE_OUTER_BOUND ( 'NONE', #14408, .T. ) ;
#19484 = PRODUCT_RELATED_PRODUCT_CATEGORY ( 'part', '', ( #6610 ) ) ;
#19485 = ORIENTED_EDGE ( 'NONE', *, *, #21315, .F. ) ;
#19486 = EDGE_LOOP ( 'NONE', ( #1421, #11710, #13549, #4986 ) ) ;
#19487 = DIRECTION ( 'NONE',  ( -1.000000000000000000, 0.000000000000000000, -0.000000000000000000 ) ) ;
#19488 = VECTOR ( 'NONE', #18543, 1000.000000000000000 ) ;
#19489 = CARTESIAN_POINT ( 'NONE',  ( -112.5606509705656464, 133.0497573896584811, -15.80384718330080140 ) ) ;
#19490 = CARTESIAN_POINT ( 'NONE',  ( 157.4999999999998579, 83.32081209086616980, 45.00000000000000000 ) ) ;
#19491 = DIRECTION ( 'NONE',  ( 0.000000000000000000, -1.000000000000000000, 0.000000000000000000 ) ) ;
#19492 = DIRECTION ( 'NONE',  ( 0.4528218681383106015, 0.8916010070293384215, -0.000000000000000000 ) ) ;
#19493 = VECTOR ( 'NONE', #6642, 1000.000000000000000 ) ;
#19494 = CARTESIAN_POINT ( 'NONE',  ( -261.1919288306253293, -171.9377729149742038, -94.99999999999987210 ) ) ;
#19495 = CARTESIAN_POINT ( 'NONE',  ( -265.0505472617491023, -165.8775750992075189, 89.59901895717871412 ) ) ;
#19496 = CARTESIAN_POINT ( 'NONE',  ( -231.9378824387722773, 93.53122965655592225, -14.99999999999998757 ) ) ;
#19497 = DIRECTION ( 'NONE',  ( 0.000000000000000000, 0.000000000000000000, 1.000000000000000000 ) ) ;
#19498 = CARTESIAN_POINT ( 'NONE',  ( 110.9201389036588949, 220.0000000000000284, 84.99999999999995737 ) ) ;
#19499 = ADVANCED_FACE ( 'NONE', ( #12556 ), #1614, .F. ) ;
#19500 = CARTESIAN_POINT ( 'NONE',  ( -175.0000000000000000, -120.0250000000001904, -63.99999999999998579 ) ) ;
#19501 = CARTESIAN_POINT ( 'NONE',  ( 150.5563491861040575, 203.0294372515228929, 45.00000000000000000 ) ) ;
#19502 = DIRECTION ( 'NONE',  ( 0.000000000000000000, 0.000000000000000000, 1.000000000000000000 ) ) ;
#19503 = VERTEX_POINT ( 'NONE', #1750 ) ;
#19504 = ADVANCED_FACE ( 'NONE', ( #17130, #25741 ), #4046, .T. ) ;
#19505 = CYLINDRICAL_SURFACE ( 'NONE', #21541, 6.000000000000032863 ) ;
#19506 = CARTESIAN_POINT ( 'NONE',  ( 157.9999999999996305, 281.6968751876750616, -45.00000000000000000 ) ) ;
#19507 = AXIS2_PLACEMENT_3D ( 'NONE', #23205, #21322, #1642 ) ;
#19508 = CARTESIAN_POINT ( 'NONE',  ( 106.9648806875826068, 209.3191036920025283, -148.6640466283485580 ) ) ;
#19509 = ORIENTED_EDGE ( 'NONE', *, *, #21537, .T. ) ;
#19510 = CIRCLE ( 'NONE', #8963, 35.00000000000000711 ) ;
#19511 = B_SPLINE_CURVE_WITH_KNOTS ( 'NONE', 3,
 ( #27506, #21048, #7707, #8123, #3380, #12450 ),
 .UNSPECIFIED., .F., .F.,
 ( 4, 2, 4 ),
 ( 0.002263534818064183874, 0.002560835764897306972, 0.002858136711730429637 ),
 .UNSPECIFIED. ) ;
#19512 = CARTESIAN_POINT ( 'NONE',  ( 97.71630809605208867, 241.5330865364702504, -11.29444388665504562 ) ) ;
#19513 = ORIENTED_EDGE ( 'NONE', *, *, #16311, .F. ) ;
#19514 = EDGE_CURVE ( 'NONE', #21211, #8565, #12834, .T. ) ;
#19515 = CARTESIAN_POINT ( 'NONE',  ( 79.99999999999991473, 140.0000000000000000, -45.00000000000000000 ) ) ;
#19516 = EDGE_LOOP ( 'NONE', ( #4871, #20478, #26289, #22310 ) ) ;
#19517 = VECTOR ( 'NONE', #20138, 1000.000000000000000 ) ;
#19518 = ORIENTED_EDGE ( 'NONE', *, *, #20317, .T. ) ;
#19519 = ADVANCED_FACE ( 'NONE', ( #21155 ), #21011, .F. ) ;
#19520 = VERTEX_POINT ( 'NONE', #21579 ) ;
#19521 = ORIENTED_EDGE ( 'NONE', *, *, #3785, .T. ) ;
#19522 = ORIENTED_EDGE ( 'NONE', *, *, #2701, .T. ) ;
#19523 = CARTESIAN_POINT ( 'NONE',  ( -12.24491960465745599, -18.01420295945611727, 95.00000000000000000 ) ) ;
#19524 = DIRECTION ( 'NONE',  ( 0.4528218681374719945, 0.8916010070297644141, -0.000000000000000000 ) ) ;
#19525 = AXIS2_PLACEMENT_3D ( 'NONE', #2060, #22174, #15300 ) ;
#19526 = AXIS2_PLACEMENT_3D ( 'NONE', #7278, #16052, #14043 ) ;
#19527 = VECTOR ( 'NONE', #8841, 1000.000000000000000 ) ;
#19528 = LINE ( 'NONE', #17363, #6119 ) ;
#19529 = EDGE_CURVE ( 'NONE', #23612, #16763, #12936, .T. ) ;
#19530 = PLANE ( 'NONE',  #12420 ) ;
#19531 = DIRECTION ( 'NONE',  ( -0.9506505318133544602, -0.3102637045530566295, 0.000000000000000000 ) ) ;
#19532 = DIRECTION ( 'NONE',  ( -0.000000000000000000, -0.000000000000000000, -1.000000000000000000 ) ) ;
#19533 = VECTOR ( 'NONE', #24056, 1000.000000000000000 ) ;
#19534 = CARTESIAN_POINT ( 'NONE',  ( 157.4999999999996589, 281.4429376839215138, 45.00000000000000000 ) ) ;
#19535 = FACE_OUTER_BOUND ( 'NONE', #15817, .T. ) ;
#19536 = EDGE_CURVE ( 'NONE', #18330, #4657, #1891, .T. ) ;
#19537 = PLANE ( 'NONE',  #21496 ) ;
#19538 = DIRECTION ( 'NONE',  ( -0.000000000000000000, -0.000000000000000000, -1.000000000000000000 ) ) ;
#19539 = DIRECTION ( 'NONE',  ( 0.4528218681373109011, -0.8916010070298462376, 0.000000000000000000 ) ) ;
#19541 = ORIENTED_EDGE ( 'NONE', *, *, #4873, .F. ) ;
#19540 = ORIENTED_EDGE ( 'NONE', *, *, #11015, .T. ) ;
#19542 = CARTESIAN_POINT ( 'NONE',  ( -170.0203570005763822, 115.7187005978582590, 25.41133611931261527 ) ) ;
#19543 = EDGE_LOOP ( 'NONE', ( #20645, #9906, #26479, #24569 ) ) ;
#19544 = SHAPE_DEFINITION_REPRESENTATION ( #17620, #10277 ) ;
#19545 = CIRCLE ( 'NONE', #22293, 5.999999999999991118 ) ;
#19546 = ORIENTED_EDGE ( 'NONE', *, *, #23405, .F. ) ;
#19547 = AXIS2_PLACEMENT_3D ( 'NONE', #5344, #17247, #28152 ) ;
#19548 = EDGE_LOOP ( 'NONE', ( #10335, #411, #12351, #12112 ) ) ;
#19549 = EDGE_CURVE ( 'NONE', #12684, #18977, #9738, .T. ) ;
#19550 = EDGE_CURVE ( 'NONE', #24175, #15078, #2455, .T. ) ;
#19551 = DIRECTION ( 'NONE',  ( -0.000000000000000000, 0.000000000000000000, 1.000000000000000000 ) ) ;
#19552 = DIRECTION ( 'NONE',  ( -0.8916010070295411483, 0.4528218681379115873, 0.000000000000000000 ) ) ;
#19553 = ORIENTED_EDGE ( 'NONE', *, *, #8706, .T. ) ;
#19554 = AXIS2_PLACEMENT_3D ( 'NONE', #25673, #1684, #25397 ) ;
#19555 = CARTESIAN_POINT ( 'NONE',  ( 90.92319367349371362, 112.0484670279546435, -100.0000000000000142 ) ) ;
#19556 = CARTESIAN_POINT ( 'NONE',  ( -175.2983697824313083, 112.8108207344445333, -27.79681538115707085 ) ) ;
#19557 = ORIENTED_EDGE ( 'NONE', *, *, #124, .F. ) ;
#19558 = CARTESIAN_POINT ( 'NONE',  ( -219.2326573687354880, 87.85061497978375655, 16.80038353493895897 ) ) ;
#19559 = ORIENTED_EDGE ( 'NONE', *, *, #3905, .F. ) ;
#19560 = CARTESIAN_POINT ( 'NONE',  ( -211.7958164186347290, -218.9496041985362922, 107.5698157934932766 ) ) ;
#19561 = EDGE_CURVE ( 'NONE', #9422, #14501, #15275, .T. ) ;
#19562 = FACE_OUTER_BOUND ( 'NONE', #19362, .T. ) ;
#19563 = DIRECTION ( 'NONE',  ( -0.8916010070298353574, 0.4528218681373319954, 0.000000000000000000 ) ) ;
#19564 = VECTOR ( 'NONE', #14578, 1000.000000000000000 ) ;
#19565 = EDGE_CURVE ( 'NONE', #12401, #12426, #20712, .T. ) ;
#19566 = PLANE ( 'NONE',  #16562 ) ;
#19567 = ORIENTED_EDGE ( 'NONE', *, *, #14204, .F. ) ;
#19568 = DIRECTION ( 'NONE',  ( 1.000000000000000000, -0.000000000000000000, -0.000000000000000000 ) ) ;
#19569 = ADVANCED_FACE ( 'NONE', ( #17548 ), #2037, .F. ) ;
#19571 = FACE_OUTER_BOUND ( 'NONE', #6888, .T. ) ;
#19570 = AXIS2_PLACEMENT_3D ( 'NONE', #13187, #8861, #11023 ) ;
#19572 = FACE_OUTER_BOUND ( 'NONE', #27366, .T. ) ;
#19573 = DIRECTION ( 'NONE',  ( -0.8916010070297548662, -0.4528218681374907573, 0.000000000000000000 ) ) ;
#19574 = ORIENTED_EDGE ( 'NONE', *, *, #20436, .F. ) ;
#19575 = CARTESIAN_POINT ( 'NONE',  ( -212.2419371577844345, -220.0000000000000853, -105.0000000000000284 ) ) ;
#19576 = CARTESIAN_POINT ( 'NONE',  ( 79.99999999999990052, 140.0000000000000000, 45.00000000000000000 ) ) ;
#19577 = CARTESIAN_POINT ( 'NONE',  ( -228.0469991721728036, 90.67060700717054544, 13.41267718625879724 ) ) ;
#19578 = ORIENTED_EDGE ( 'NONE', *, *, #9523, .T. ) ;
#19579 =( NAMED_UNIT ( * ) PLANE_ANGLE_UNIT ( ) SI_UNIT ( $, .RADIAN. ) );
#19580 = EDGE_LOOP ( 'NONE', ( #2057, #4627, #7103, #15474 ) ) ;
#19581 = CARTESIAN_POINT ( 'NONE',  ( 157.9999999999996589, 276.1732501651540588, 45.00000000000000000 ) ) ;
#19582 = CARTESIAN_POINT ( 'NONE',  ( -169.6922851464237567, 115.8923280138696157, -26.07704740418152767 ) ) ;
#19583 = ORIENTED_EDGE ( 'NONE', *, *, #6653, .T. ) ;
#19584 = ADVANCED_FACE ( 'NONE', ( #17836 ), #175, .T. ) ;
#19585 = AXIS2_PLACEMENT_3D ( 'NONE', #23269, #1569, #25551 ) ;
#19586 = ORIENTED_EDGE ( 'NONE', *, *, #15186, .T. ) ;
#19587 = DIRECTION ( 'NONE',  ( 0.7071067811865474617, 8.659560562354932858E-17, 0.7071067811865474617 ) ) ;
#19588 = CIRCLE ( 'NONE', #14551, 5.999999999999977796 ) ;
#19589 = CARTESIAN_POINT ( 'NONE',  ( 142.6536686473019699, 201.5224093497741649, -45.00000000000000000 ) ) ;
#19590 = ORIENTED_EDGE ( 'NONE', *, *, #1286, .F. ) ;
#19591 = ORIENTED_EDGE ( 'NONE', *, *, #19596, .F. ) ;
#19592 = CARTESIAN_POINT ( 'NONE',  ( -23.60339304038094710, 128.1103613223097284, 17.45643390080418911 ) ) ;
#19593 = CARTESIAN_POINT ( 'NONE',  ( -225.7036482868739427, -91.18033988749901653, 18.91107291867258766 ) ) ;
#19594 = CARTESIAN_POINT ( 'NONE',  ( -160.0000000000000284, 79.99999999999994316, -100.0000000000000142 ) ) ;
#19595 = DIRECTION ( 'NONE',  ( 0.9682458365518546994, -0.000000000000000000, 0.2499999999999989453 ) ) ;
#19596 = EDGE_CURVE ( 'NONE', #7880, #18534, #4333, .T. ) ;
#19597 = EDGE_CURVE ( 'NONE', #20740, #17150, #19847, .T. ) ;
#19598 = CYLINDRICAL_SURFACE ( 'NONE', #9205, 166.0121251338587172 ) ;
#19599 = CARTESIAN_POINT ( 'NONE',  ( 157.9999999999999716, 208.9684999699701393, 45.00000000000000000 ) ) ;
#19600 = CARTESIAN_POINT ( 'NONE',  ( -225.5840809296905149, 72.49952595022725177, -18.07266724760468080 ) ) ;
#19601 = EDGE_LOOP ( 'NONE', ( #5866, #11970, #379, #23970, #6293, #25169 ) ) ;
#19602 = DIRECTION ( 'NONE',  ( -0.5975062131282553590, 0.8018642810807399268, 0.000000000000000000 ) ) ;
#19603 = CARTESIAN_POINT ( 'NONE',  ( 157.9999999999996589, 274.1732501651540588, 45.00000000000000000 ) ) ;
#19604 = LINE ( 'NONE', #28343, #21975 ) ;
#19605 = CARTESIAN_POINT ( 'NONE',  ( 114.6860526936810487, 229.7243539224658093, -98.48425370696855907 ) ) ;
#19606 = AXIS2_PLACEMENT_3D ( 'NONE', #20150, #18003, #21134 ) ;
#19607 = ORIENTED_EDGE ( 'NONE', *, *, #983, .F. ) ;
#19608 = CARTESIAN_POINT ( 'NONE',  ( 158.0000000000008242, 128.2086247222394206, 45.00000000000000000 ) ) ;
#19609 = DIRECTION ( 'NONE',  ( 0.05364526231778203591, -0.9985600561963492439, 0.000000000000000000 ) ) ;
#19610 = CARTESIAN_POINT ( 'NONE',  ( 282.4999999999996589, 19.41075299063184900, 87.99671038392668265 ) ) ;
#19611 = CARTESIAN_POINT ( 'NONE',  ( 158.0000000000001421, 191.4133749174225443, -45.00000000000000000 ) ) ;
#19612 = CARTESIAN_POINT ( 'NONE',  ( 158.0000000000015348, 58.49599951954928656, 45.00000000000000000 ) ) ;
#19613 =( NAMED_UNIT ( * ) SI_UNIT ( $, .STERADIAN. ) SOLID_ANGLE_UNIT ( ) );
#19614 = ORIENTED_EDGE ( 'NONE', *, *, #27460, .F. ) ;
#19615 = CARTESIAN_POINT ( 'NONE',  ( 115.6411010564592061, 231.4666050640012998, 99.00000000000001421 ) ) ;
#19616 = ORIENTED_EDGE ( 'NONE', *, *, #7014, .T. ) ;
#19617 = EDGE_CURVE ( 'NONE', #24242, #12999, #26025, .T. ) ;
#19618 = CARTESIAN_POINT ( 'NONE',  ( -266.7059280454142822, -170.8119893264861844, 94.52701477642899874 ) ) ;
#19619 = ORIENTED_EDGE ( 'NONE', *, *, #7580, .F. ) ;
#19620 = ORIENTED_EDGE ( 'NONE', *, *, #7862, .T. ) ;
#19621 = CARTESIAN_POINT ( 'NONE',  ( -221.3650667873343139, -91.18033988749901653, 19.29759039828519818 ) ) ;
#19622 = AXIS2_PLACEMENT_3D ( 'NONE', #8365, #23446, #19134 ) ;
#19623 = EDGE_CURVE ( 'NONE', #5842, #4420, #12958, .T. ) ;
#19624 = VERTEX_POINT ( 'NONE', #19707 ) ;
#19625 = ORIENTED_EDGE ( 'NONE', *, *, #16246, .F. ) ;
#19626 = CARTESIAN_POINT ( 'NONE',  ( -217.6530384384126080, 140.9974917369520426, 15.00000000000000000 ) ) ;
#19627 = AXIS2_PLACEMENT_3D ( 'NONE', #6869, #11771, #2550 ) ;
#19628 = CARTESIAN_POINT ( 'NONE',  ( -107.6076100521348877, 133.6773311915829936, -15.67055231630294010 ) ) ;
#19629 = CARTESIAN_POINT ( 'NONE',  ( 157.9999999999998579, 223.5078750075070104, 45.00000000000000000 ) ) ;
#19630 = CYLINDRICAL_SURFACE ( 'NONE', #1816, 30.00000000000002842 ) ;
#19631 = EDGE_CURVE ( 'NONE', #24933, #1342, #18915, .T. ) ;
#19632 = DIRECTION ( 'NONE',  ( -0.8916010070298556744, 0.4528218681372921939, 0.000000000000000000 ) ) ;
#19633 = EDGE_CURVE ( 'NONE', #9022, #19307, #31, .T. ) ;
#19634 = CARTESIAN_POINT ( 'NONE',  ( 158.0000000000013074, 81.06687458711267880, 45.00000000000000000 ) ) ;
#19635 = DIRECTION ( 'NONE',  ( -0.05364526231779760679, -0.9985600561963485777, 0.000000000000000000 ) ) ;
#19636 = CARTESIAN_POINT ( 'NONE',  ( -212.5754918423282618, 87.16543701462498461, -23.36890611379539706 ) ) ;
#19637 = ADVANCED_FACE ( 'NONE', ( #19572 ), #8790, .F. ) ;
#19638 = DIRECTION ( 'NONE',  ( 0.000000000000000000, 1.000000000000000000, 0.000000000000000000 ) ) ;
#19639 = DIRECTION ( 'NONE',  ( -0.000000000000000000, -0.000000000000000000, 1.000000000000000000 ) ) ;
#19640 = DIRECTION ( 'NONE',  ( -0.000000000000000000, -0.000000000000000000, -1.000000000000000000 ) ) ;
#19641 = CARTESIAN_POINT ( 'NONE',  ( -140.1213116003368668, 122.5384136796733827, 12.99999999999999822 ) ) ;
#19642 = ORIENTED_EDGE ( 'NONE', *, *, #9397, .T. ) ;
#19643 = PLANE ( 'NONE',  #10133 ) ;
#19644 = VECTOR ( 'NONE', #19075, 1000.000000000000000 ) ;
#19645 = VECTOR ( 'NONE', #11090, 1000.000000000000000 ) ;
#19646 = CARTESIAN_POINT ( 'NONE',  ( -141.6428522700808230, 22.24192588826928585, 83.00000000000001421 ) ) ;
#19647 = CYLINDRICAL_SURFACE ( 'NONE', #26816, 30.00000000000000000 ) ;
#19648 = DIRECTION ( 'NONE',  ( -1.000000000000000000, 0.000000000000000000, -0.000000000000000000 ) ) ;
#19649 = EDGE_LOOP ( 'NONE', ( #11223, #17111, #12046, #13538 ) ) ;
#19650 = CARTESIAN_POINT ( 'NONE',  ( 92.49170488791030209, 239.7529794472836215, -17.61766721977555505 ) ) ;
#19651 = ORIENTED_EDGE ( 'NONE', *, *, #25383, .F. ) ;
#19652 = CARTESIAN_POINT ( 'NONE',  ( -20.35978069378271726, 129.6268764493030687, -15.48139849003159618 ) ) ;
#19653 = VERTEX_POINT ( 'NONE', #15414 ) ;
#19654 = ORIENTED_EDGE ( 'NONE', *, *, #3438, .F. ) ;
#19655 = AXIS2_PLACEMENT_3D ( 'NONE', #17030, #12035, #23082 ) ;
#19656 = VERTEX_POINT ( 'NONE', #2312 ) ;
#19657 = VERTEX_POINT ( 'NONE', #24169 ) ;
#19658 = ORIENTED_EDGE ( 'NONE', *, *, #7639, .F. ) ;
#19659 = CARTESIAN_POINT ( 'NONE',  ( 158.0000000000011653, 95.60624962464788723, -45.00000000000000000 ) ) ;
#19660 = ADVANCED_FACE ( 'NONE', ( #15128 ), #13258, .F. ) ;
#19661 = CIRCLE ( 'NONE', #28352, 562.1290781602208426 ) ;
#19662 = ADVANCED_FACE ( 'NONE', ( #15552 ), #24302, .T. ) ;
#19663 = VECTOR ( 'NONE', #5571, 1000.000000000000114 ) ;
#19664 = LINE ( 'NONE', #15370, #21549 ) ;
#19665 = LINE ( 'NONE', #9037, #1986 ) ;
#19666 = CARTESIAN_POINT ( 'NONE',  ( -226.0190876347067785, 72.67478414371682049, 17.85134081709900755 ) ) ;
#19667 = DIRECTION ( 'NONE',  ( 0.4528218681380115629, 0.8916010070294903000, -0.000000000000000000 ) ) ;
#19668 = FACE_OUTER_BOUND ( 'NONE', #26002, .T. ) ;
#19669 = ADVANCED_FACE ( 'NONE', ( #13542 ), #25334, .T. ) ;
#19670 = LINE ( 'NONE', #4432, #19082 ) ;
#19671 = CARTESIAN_POINT ( 'NONE',  ( 157.9999999999998010, 236.0472500450420341, 45.00000000000000000 ) ) ;
#19672 = CARTESIAN_POINT ( 'NONE',  ( 79.99999999999992895, 230.0000000000000000, 5.000000000000002665 ) ) ;
#19673 = DIRECTION ( 'NONE',  ( 0.000000000000000000, 0.000000000000000000, 1.000000000000000000 ) ) ;
#19674 = EDGE_CURVE ( 'NONE', #17424, #9868, #2604, .T. ) ;
#19676 = VECTOR ( 'NONE', #20276, 1000.000000000000114 ) ;
#19675 = CARTESIAN_POINT ( 'NONE',  ( 232.4999999999996305, 83.06687458711267880, 42.86484227207692754 ) ) ;
#19677 = CARTESIAN_POINT ( 'NONE',  ( -209.9813605129777159, 61.38896102042362912, 24.60123923356250586 ) ) ;
#19678 = CARTESIAN_POINT ( 'NONE',  ( -210.0000000000000000, -150.0000000000001990, 100.0000000000000142 ) ) ;
#19679 = DIRECTION ( 'NONE',  ( 0.000000000000000000, -1.000000000000000000, 0.000000000000000000 ) ) ;
#19681 = ORIENTED_EDGE ( 'NONE', *, *, #4030, .T. ) ;
#19680 = ORIENTED_EDGE ( 'NONE', *, *, #1284, .F. ) ;
#19682 = CARTESIAN_POINT ( 'NONE',  ( -169.7566311317153236, 115.8586538395105237, 26.10480086864442839 ) ) ;
#19683 = AXIS2_PLACEMENT_3D ( 'NONE', #3808, #10847, #19319 ) ;
#19684 = PRODUCT ( 'MAS-315', 'MAS-315', '', ( #10077 ) ) ;
#19685 = PLANE ( 'NONE',  #18612 ) ;
#19686 = ORIENTED_EDGE ( 'NONE', *, *, #25815, .F. ) ;
#19687 = CONTEXT_DEPENDENT_SHAPE_REPRESENTATION ( #10938, #10497 ) ;
#19688 = ORIENTED_EDGE ( 'NONE', *, *, #16788, .F. ) ;
#19689 = ORIENTED_EDGE ( 'NONE', *, *, #8874, .T. ) ;
#19690 = DIRECTION ( 'NONE',  ( 0.000000000000000000, -1.214306433183764966E-16, 1.000000000000000000 ) ) ;
#19691 = DIRECTION ( 'NONE',  ( 0.000000000000000000, 0.000000000000000000, -1.000000000000000000 ) ) ;
#19692 = VERTEX_POINT ( 'NONE', #22725 ) ;
#19693 = CARTESIAN_POINT ( 'NONE',  ( 119.9999999999999147, 140.0000000000000000, -100.0000000000000142 ) ) ;
#19694 = EDGE_CURVE ( 'NONE', #12920, #22238, #747, .T. ) ;
#19695 = AXIS2_PLACEMENT_3D ( 'NONE', #3771, #23601, #21300 ) ;
#19696 = DIRECTION ( 'NONE',  ( -0.000000000000000000, -0.000000000000000000, 1.000000000000000000 ) ) ;
#19697 = ORIENTED_EDGE ( 'NONE', *, *, #16904, .F. ) ;
#19698 = CARTESIAN_POINT ( 'NONE',  ( -211.8433833244381503, 88.46778497223422733, 21.92823303506064292 ) ) ;
#19699 = VERTEX_POINT ( 'NONE', #16125 ) ;
#19700 = CARTESIAN_POINT ( 'NONE',  ( -213.1553235149991110, -216.8625818769947955, 105.0933958169749047 ) ) ;
#19701 = DIRECTION ( 'NONE',  ( 0.000000000000000000, 1.000000000000000000, 0.000000000000000000 ) ) ;
#19702 = CARTESIAN_POINT ( 'NONE',  ( 160.2722134808911107, 203.8336097610383035, -150.8460904732142751 ) ) ;
#19703 = VERTEX_POINT ( 'NONE', #22858 ) ;
#19704 = EDGE_CURVE ( 'NONE', #21239, #991, #7213, .T. ) ;
#19705 = EDGE_CURVE ( 'NONE', #12605, #4176, #20278, .T. ) ;
#19706 = DIRECTION ( 'NONE',  ( -1.000000000000000000, -0.000000000000000000, 0.000000000000000000 ) ) ;
#19707 = CARTESIAN_POINT ( 'NONE',  ( 330.9869376377542949, 44.41075299063184190, 75.35061095560295996 ) ) ;
#19708 = DIRECTION ( 'NONE',  ( 0.000000000000000000, -1.000000000000000000, -1.214306433183764966E-16 ) ) ;
#19709 = ORIENTED_EDGE ( 'NONE', *, *, #20357, .T. ) ;
#19710 = DIRECTION ( 'NONE',  ( 1.000000000000000000, 0.000000000000000000, 0.000000000000000000 ) ) ;
#19711 = VECTOR ( 'NONE', #15669, 1000.000000000000000 ) ;
#19712 = DIRECTION ( 'NONE',  ( 0.000000000000000000, -1.000000000000000000, 0.000000000000000000 ) ) ;
#19713 = CARTESIAN_POINT ( 'NONE',  ( -180.0000000000000284, -2.775557561562891982E-14, -100.0000000000000142 ) ) ;
#19714 = ORIENTED_EDGE ( 'NONE', *, *, #10651, .F. ) ;
#19715 = ORIENTED_EDGE ( 'NONE', *, *, #4736, .F. ) ;
#19716 = ADVANCED_FACE ( 'NONE', ( #1020 ), #27295, .F. ) ;
#19717 = AXIS2_PLACEMENT_3D ( 'NONE', #19746, #2353, #8274 ) ;
#19718 = ADVANCED_FACE ( 'NONE', ( #7066, #7635 ), #25147, .T. ) ;
#19719 = CARTESIAN_POINT ( 'NONE',  ( 157.9999999999998863, 216.4921249924925348, 45.00000000000000000 ) ) ;
#19720 = CARTESIAN_POINT ( 'NONE',  ( -186.8149004422502912, 105.6021380271806436, -32.12667098497705354 ) ) ;
#19721 = VERTEX_POINT ( 'NONE', #17986 ) ;
#19722 = ORIENTED_EDGE ( 'NONE', *, *, #24148, .T. ) ;
#19723 = DIRECTION ( 'NONE',  ( 0.6787614006938652578, 0.7343588774761984350, 0.000000000000000000 ) ) ;
#19724 = CARTESIAN_POINT ( 'NONE',  ( 217.4999999999996305, -5.589247009368160768, 100.0000000000000142 ) ) ;
#19725 = EDGE_CURVE ( 'NONE', #17425, #16662, #21208, .T. ) ;
#19726 = ORIENTED_EDGE ( 'NONE', *, *, #25863, .T. ) ;
#19727 = ORIENTED_EDGE ( 'NONE', *, *, #14586, .T. ) ;
#19728 = CARTESIAN_POINT ( 'NONE',  ( -28.22105481086200385, 127.9579655952397275, 17.52291750101008105 ) ) ;
#19729 = CIRCLE ( 'NONE', #12859, 5.999999999999977796 ) ;
#19730 = CARTESIAN_POINT ( 'NONE',  ( -160.0000000000000284, 59.99999999999994316, 70.00000000000001421 ) ) ;
#19731 = DIRECTION ( 'NONE',  ( -0.2588190451025286221, -0.9659258262890662028, 0.000000000000000000 ) ) ;
#19732 = DIRECTION ( 'NONE',  ( 1.000000000000000000, -0.000000000000000000, -0.000000000000000000 ) ) ;
#19733 = DIRECTION ( 'NONE',  ( 0.000000000000000000, 0.000000000000000000, 1.000000000000000000 ) ) ;
#19734 = DIRECTION ( 'NONE',  ( 1.000000000000000000, 0.000000000000000000, 0.000000000000000000 ) ) ;
#19735 = CIRCLE ( 'NONE', #27085, 19.68410787789781580 ) ;
#19736 = CARTESIAN_POINT ( 'NONE',  ( 144.9999999999998863, 220.0000000000000284, 45.00000000000000000 ) ) ;
#19737 = EDGE_LOOP ( 'NONE', ( #22162, #7150, #8395, #3112, #14329, #22208, #26662, #14687 ) ) ;
#19738 = LINE ( 'NONE', #10987, #5876 ) ;
#19739 = PLANE ( 'NONE',  #6503 ) ;
#19740 = DIRECTION ( 'NONE',  ( 0.8916010070293682865, 0.4528218681382519262, 0.000000000000000000 ) ) ;
#19741 = LINE ( 'NONE', #26343, #19428 ) ;
#19742 = VERTEX_POINT ( 'NONE', #15986 ) ;
#19743 = DIRECTION ( 'NONE',  ( 0.000000000000000000, 0.000000000000000000, -1.000000000000000000 ) ) ;
#19744 = VERTEX_POINT ( 'NONE', #11538 ) ;
#19745 = DIRECTION ( 'NONE',  ( 0.000000000000000000, -1.000000000000000000, 0.000000000000000000 ) ) ;
#19746 = CARTESIAN_POINT ( 'NONE',  ( -63.57415822541634043, 75.97823757117562593, 95.00000000000000000 ) ) ;
#19747 = CARTESIAN_POINT ( 'NONE',  ( 217.4999999999996305, -5.589247009368136787, -100.0000000000000142 ) ) ;
#19748 = LINE ( 'NONE', #25930, #23929 ) ;
#19749 = DIRECTION ( 'NONE',  ( 1.000000000000000000, -0.000000000000000000, -0.000000000000000000 ) ) ;
#19750 = ORIENTED_EDGE ( 'NONE', *, *, #24823, .T. ) ;
#19751 = VECTOR ( 'NONE', #2775, 1000.000000000000227 ) ;
#19752 = CARTESIAN_POINT ( 'NONE',  ( 158.0000000000002274, 185.8897498949014278, 45.00000000000000000 ) ) ;
#19753 = ORIENTED_EDGE ( 'NONE', *, *, #508, .T. ) ;
#19754 = CARTESIAN_POINT ( 'NONE',  ( -272.1218244932625225, -170.1898742340911781, 92.97996575210989079 ) ) ;
#19755 = VERTEX_POINT ( 'NONE', #3027 ) ;
#19756 = EDGE_CURVE ( 'NONE', #7140, #27404, #2393, .T. ) ;
#19757 = EDGE_LOOP ( 'NONE', ( #25751, #15204, #21242, #25945 ) ) ;
#19758 = ADVANCED_FACE ( 'NONE', ( #5467 ), #11817, .F. ) ;
#19759 = DIRECTION ( 'NONE',  ( 0.4528218681371909971, -0.8916010070299070778, 0.000000000000000000 ) ) ;
#19760 = CONICAL_SURFACE ( 'NONE', #19289, 6.025000000000002132, 0.7853981633971707232 ) ;
#19761 = ADVANCED_FACE ( 'NONE', ( #24875 ), #20417, .F. ) ;
#19762 = ORIENTED_EDGE ( 'NONE', *, *, #21141, .T. ) ;
#19763 = ORIENTED_EDGE ( 'NONE', *, *, #3549, .T. ) ;
#19764 = CARTESIAN_POINT ( 'NONE',  ( -225.9729034214342676, 132.4331356209129638, 12.99353264123212526 ) ) ;
#19765 = CARTESIAN_POINT ( 'NONE',  ( 96.93828241645127264, 232.7455409703985936, 20.22303902613926851 ) ) ;
#19766 = DIRECTION ( 'NONE',  ( -0.9784193629480785193, 0.2066290158914672603, 0.000000000000000000 ) ) ;
#19767 = CARTESIAN_POINT ( 'NONE',  ( -305.0000000000001137, -170.0000000000001137, -59.99999999999987210 ) ) ;
#19768 = DIRECTION ( 'NONE',  ( -0.000000000000000000, 0.000000000000000000, -1.000000000000000000 ) ) ;
#19769 = DIRECTION ( 'NONE',  ( 0.8916010070296429557, -0.4528218681377111920, 0.000000000000000000 ) ) ;
#19770 = FACE_OUTER_BOUND ( 'NONE', #9975, .T. ) ;
#19771 = VECTOR ( 'NONE', #4040, 999.9999999999998863 ) ;
#19772 = LINE ( 'NONE', #15484, #28268 ) ;
#19773 = FACE_OUTER_BOUND ( 'NONE', #13038, .T. ) ;
#19774 = DIRECTION ( 'NONE',  ( 0.000000000000000000, 1.000000000000000000, 0.000000000000000000 ) ) ;
#19775 = FACE_OUTER_BOUND ( 'NONE', #10086, .T. ) ;
#19776 = DIRECTION ( 'NONE',  ( -0.000000000000000000, -0.000000000000000000, -1.000000000000000000 ) ) ;
#19777 = ORIENTED_EDGE ( 'NONE', *, *, #14454, .F. ) ;
#19778 = DIRECTION ( 'NONE',  ( 1.000000000000000000, 0.000000000000000000, -0.000000000000000000 ) ) ;
#19779 = VECTOR ( 'NONE', #22404, 1000.000000000000000 ) ;
#19780 = EDGE_CURVE ( 'NONE', #268, #22186, #2857, .T. ) ;
#19781 = DIRECTION ( 'NONE',  ( 0.4528218681383305855, -0.8916010070293283185, 0.000000000000000000 ) ) ;
#19782 = DIRECTION ( 'NONE',  ( 0.000000000000000000, -0.000000000000000000, -1.000000000000000000 ) ) ;
#19783 = DIRECTION ( 'NONE',  ( -0.000000000000000000, -0.000000000000000000, -1.000000000000000000 ) ) ;
#19784 = ORIENTED_EDGE ( 'NONE', *, *, #5128, .T. ) ;
#19785 = CARTESIAN_POINT ( 'NONE',  ( 157.4999999999994600, 216.2381874887387880, 45.00000000000000000 ) ) ;
#19786 = ORIENTED_EDGE ( 'NONE', *, *, #12227, .T. ) ;
#19787 = CARTESIAN_POINT ( 'NONE',  ( -7.443569385156187046, 132.8772577174391643, -14.28756630290005525 ) ) ;
#19788 = ORIENTED_EDGE ( 'NONE', *, *, #866, .T. ) ;
#19789 = EDGE_CURVE ( 'NONE', #4776, #3728, #2745, .T. ) ;
#19790 = VERTEX_POINT ( 'NONE', #14249 ) ;
#19791 = EDGE_CURVE ( 'NONE', #8030, #27317, #9763, .T. ) ;
#19792 = EDGE_CURVE ( 'NONE', #8705, #5655, #22583, .T. ) ;
#19793 = VECTOR ( 'NONE', #23074, 1000.000000000000000 ) ;
#19794 = EDGE_CURVE ( 'NONE', #23572, #7620, #25016, .T. ) ;
#19795 = VERTEX_POINT ( 'NONE', #14108 ) ;
#19796 = ORIENTED_EDGE ( 'NONE', *, *, #23003, .T. ) ;
#19797 = CARTESIAN_POINT ( 'NONE',  ( 158.0000000000011653, 95.60624962464788723, -45.00000000000000000 ) ) ;
#19798 = AXIS2_PLACEMENT_3D ( 'NONE', #3071, #9270, #13879 ) ;
#19799 = LINE ( 'NONE', #14937, #3561 ) ;
#19800 = AXIS2_PLACEMENT_3D ( 'NONE', #3985, #25825, #12491 ) ;
#19801 = LINE ( 'NONE', #21822, #13279 ) ;
#19802 = UNCERTAINTY_MEASURE_WITH_UNIT (LENGTH_MEASURE( 1.000000000000000082E-05 ), #6958, 'distance_accuracy_value', 'NONE');
#19803 = DIRECTION ( 'NONE',  ( 0.000000000000000000, 0.000000000000000000, -1.000000000000000000 ) ) ;
#19804 = CARTESIAN_POINT ( 'NONE',  ( -220.9458266506729842, 71.36862438102525630, 20.99673689147903843 ) ) ;
#19805 = CARTESIAN_POINT ( 'NONE',  ( 157.4999999999998579, 55.73418700828869277, 45.00000000000000000 ) ) ;
#19806 = PLANE ( 'NONE',  #19989 ) ;
#19807 = DIRECTION ( 'NONE',  ( -0.8018642810807398158, -0.5975062131282554700, 0.000000000000000000 ) ) ;
#19808 = DIRECTION ( 'NONE',  ( 0.000000000000000000, 0.000000000000000000, -1.000000000000000000 ) ) ;
#19809 = CYLINDRICAL_SURFACE ( 'NONE', #21919, 5.999999999999977796 ) ;
#19810 = CARTESIAN_POINT ( 'NONE',  ( 33.10302365956999182, 221.6666220619077876, 15.00000000000000000 ) ) ;
#19811 = AXIS2_PLACEMENT_3D ( 'NONE', #5926, #23453, #14700 ) ;
#19812 = CARTESIAN_POINT ( 'NONE',  ( -40.77177304839534600, 129.1844851112595904, 17.01161629403331688 ) ) ;
#19813 = CARTESIAN_POINT ( 'NONE',  ( -209.9947863080667787, 60.75003584150559988, 22.65371792907697568 ) ) ;
#19814 = CARTESIAN_POINT ( 'NONE',  ( 217.4749999999996533, 258.6181251126050711, 1.387778780781445676E-14 ) ) ;
#19815 = CARTESIAN_POINT ( 'NONE',  ( 158.0000000000014211, 70.52749954957745615, -45.00000000000000000 ) ) ;
#19816 = VECTOR ( 'NONE', #21310, 1000.000000000000000 ) ;
#19818 = ORIENTED_EDGE ( 'NONE', *, *, #10209, .T. ) ;
#19817 = ORIENTED_EDGE ( 'NONE', *, *, #1538, .F. ) ;
#19819 = CARTESIAN_POINT ( 'NONE',  ( -175.1909440597360117, 112.8732459110917006, 28.42595730244120134 ) ) ;
#19820 = ADVANCED_FACE ( 'NONE', ( #20695 ), #11386, .F. ) ;
#19821 = PRESENTATION_LAYER_ASSIGNMENT (  '', '', ( #14790 ) ) ;
#19822 = ADVANCED_FACE ( 'NONE', ( #1300 ), #6177, .F. ) ;
#19823 = CARTESIAN_POINT ( 'NONE',  ( -205.5903157496420022, 91.23080130178013292, -28.02187135762362757 ) ) ;
#19824 = ORIENTED_EDGE ( 'NONE', *, *, #22541, .T. ) ;
#19825 = ORIENTED_EDGE ( 'NONE', *, *, #2013, .T. ) ;
#19826 = ORIENTED_EDGE ( 'NONE', *, *, #9716, .T. ) ;
#19827 = EDGE_CURVE ( 'NONE', #2081, #6570, #14954, .T. ) ;
#19828 = DIRECTION ( 'NONE',  ( 0.000000000000000000, 0.000000000000000000, 1.000000000000000000 ) ) ;
#19829 = CARTESIAN_POINT ( 'NONE',  ( -113.0182548846454011, 134.5412002400303209, 13.86291542401011156 ) ) ;
#19830 = EDGE_CURVE ( 'NONE', #13130, #26005, #1436, .T. ) ;
#19831 = ORIENTED_EDGE ( 'NONE', *, *, #25718, .T. ) ;
#19832 =( BOUNDED_SURFACE ( )  B_SPLINE_SURFACE ( 3, 2, ( 
 ( #9999, #5116, #25365 ),
 ( #20912, #20349, #22656 ),
 ( #14315, #27094, #2815 ),
 ( #817, #3095, #14047 ),
 ( #12024, #5541, #12169 ),
 ( #9721, #3236, #27505 ),
 ( #681, #13908, #24807 ),
 ( #2963, #11753, #20769 ) ),
 .UNSPECIFIED., .F., .F., .F. ) 
 B_SPLINE_SURFACE_WITH_KNOTS ( ( 4, 2, 2, 4 ),
 ( 3, 3 ),
 ( 0.000000000000000000, 0.008853367702742013026, 0.01328005155411302041, 0.01770673540548402605 ),
 ( 0.000000000000000000, 1.000000000000000000 ),
 .UNSPECIFIED. ) 
 GEOMETRIC_REPRESENTATION_ITEM ( )  RATIONAL_B_SPLINE_SURFACE ( (
 ( 1.000000000000000000, 0.7071067811865475727, 1.000000000000000000),
 ( 1.000000000000000000, 0.7122833902602503375, 1.000000000000000000),
 ( 1.000000000000000000, 0.7150365851228822622, 1.000000000000000000),
 ( 1.000000000000000000, 0.7151618057631559111, 1.000000000000000000),
 ( 1.000000000000000000, 0.7145339593740676065, 1.000000000000000000),
 ( 1.000000000000000000, 0.7118598333332957218, 1.000000000000000000),
 ( 1.000000000000000000, 0.7098294805783303962, 1.000000000000000000),
 ( 1.000000000000000000, 0.7071067811865465735, 1.000000000000000000) ) ) 
 REPRESENTATION_ITEM ( '' )  SURFACE ( )  );
#19833 = VECTOR ( 'NONE', #17855, 1000.000000000000000 ) ;
#19834 = CARTESIAN_POINT ( 'NONE',  ( 100.8904249506145874, 86.57652225509636423, -100.0000000000000142 ) ) ;
#19835 = VECTOR ( 'NONE', #19108, 1000.000000000000000 ) ;
#19836 = CARTESIAN_POINT ( 'NONE',  ( 134.9999999999998579, 244.8793018922092699, -151.0000000000000284 ) ) ;
#19837 = VERTEX_POINT ( 'NONE', #6032 ) ;
#19838 = CARTESIAN_POINT ( 'NONE',  ( -224.3954463207928711, 86.96133147683917741, 16.77313708869839104 ) ) ;
#19839 = AXIS2_PLACEMENT_3D ( 'NONE', #9997, #11749, #22793 ) ;
#19840 = CARTESIAN_POINT ( 'NONE',  ( -260.0000000000001137, -152.0000000000000284, -104.9999999999998721 ) ) ;
#19841 = AXIS2_PLACEMENT_3D ( 'NONE', #5726, #859, #14503 ) ;
#19842 = DIRECTION ( 'NONE',  ( -1.000000000000000000, 0.000000000000000000, -2.220446049250266932E-15 ) ) ;
#19843 = CARTESIAN_POINT ( 'NONE',  ( 157.8683049041797517, 200.5822371829430040, -142.3407963099403446 ) ) ;
#19844 = VERTEX_POINT ( 'NONE', #18823 ) ;
#19845 = CARTESIAN_POINT ( 'NONE',  ( -270.1025481742786951, -91.18033988749901653, 0.000000000000000000 ) ) ;
#19846 = DIRECTION ( 'NONE',  ( 1.000000000000000000, -0.000000000000000000, -0.000000000000000000 ) ) ;
#19847 = LINE ( 'NONE', #4190, #15257 ) ;
#19848 = CARTESIAN_POINT ( 'NONE',  ( 330.9869376377542949, 44.41075299063183479, -100.0000000000000284 ) ) ;
#19849 = ORIENTED_EDGE ( 'NONE', *, *, #3116, .F. ) ;
#19850 = CIRCLE ( 'NONE', #11120, 30.00000000000002842 ) ;
#19851 = CARTESIAN_POINT ( 'NONE',  ( 157.4999999999998579, 178.6200623761337738, 45.00000000000000000 ) ) ;
#19852 = EDGE_CURVE ( 'NONE', #26795, #21098, #8336, .T. ) ;
#19853 = AXIS2_PLACEMENT_3D ( 'NONE', #15172, #9904, #2076 ) ;
#19854 = CARTESIAN_POINT ( 'NONE',  ( 209.9999999999999432, 0.000000000000000000, -99.99999999999995737 ) ) ;
#19855 = CARTESIAN_POINT ( 'NONE',  ( -160.0000000000000568, 230.0000000000000000, -15.00000000000000000 ) ) ;
#19856 = ORIENTED_EDGE ( 'NONE', *, *, #11305, .T. ) ;
#19857 = CARTESIAN_POINT ( 'NONE',  ( 0.000000000000000000, 0.000000000000000000, 0.000000000000000000 ) ) ;
#19858 = AXIS2_PLACEMENT_3D ( 'NONE', #9619, #2996, #13946 ) ;
#19859 = ORIENTED_EDGE ( 'NONE', *, *, #20508, .T. ) ;
#19860 = CARTESIAN_POINT ( 'NONE',  ( 158.0000000000010800, 101.1298746471690038, 45.00000000000000000 ) ) ;
#19861 = CARTESIAN_POINT ( 'NONE',  ( -196.6299573648443868, 98.19963181860228474, -32.16283524453812959 ) ) ;
#19862 = ORIENTED_EDGE ( 'NONE', *, *, #25795, .F. ) ;
#19863 = ORIENTED_EDGE ( 'NONE', *, *, #19351, .F. ) ;
#19864 = PLANE ( 'NONE',  #3050 ) ;
#19865 = EDGE_CURVE ( 'NONE', #25224, #22406, #25290, .T. ) ;
#19866 = DIRECTION ( 'NONE',  ( -1.000000000000000000, -0.000000000000000000, -0.000000000000000000 ) ) ;
#19867 = EDGE_LOOP ( 'NONE', ( #13873, #16514, #12047, #6611 ) ) ;
#19868 = ORIENTED_EDGE ( 'NONE', *, *, #25013, .F. ) ;
#19869 = AXIS2_PLACEMENT_3D ( 'NONE', #26611, #17572, #26331 ) ;
#19870 = CARTESIAN_POINT ( 'NONE',  ( 134.9999999999998579, 220.0000000000000284, -100.0000000000000142 ) ) ;
#19871 = VECTOR ( 'NONE', #13128, 1000.000000000000114 ) ;
#19872 = LINE ( 'NONE', #11265, #4834 ) ;
#19873 = CARTESIAN_POINT ( 'NONE',  ( 167.4999999999996589, 526.4263741777961059, 84.99999999999995737 ) ) ;
#19874 = DIRECTION ( 'NONE',  ( 0.000000000000000000, -1.000000000000000000, 0.000000000000000000 ) ) ;
#19875 = CIRCLE ( 'NONE', #12086, 30.00000000000000711 ) ;
#19876 = CARTESIAN_POINT ( 'NONE',  ( 158.0000000000013358, 80.55899957960563995, -45.00000000000000000 ) ) ;
#19877 = EDGE_CURVE ( 'NONE', #17145, #14062, #23418, .T. ) ;
#19878 = CARTESIAN_POINT ( 'NONE',  ( 158.0000000000015632, 57.98812451204224061, 45.00000000000000000 ) ) ;
#19879 = SPHERICAL_SURFACE ( 'NONE', #26567, 5.000000000000000000 ) ;
#19880 = ORIENTED_EDGE ( 'NONE', *, *, #4216, .T. ) ;
#19881 = ADVANCED_FACE ( 'NONE', ( #3586 ), #10203, .T. ) ;
#19882 = CARTESIAN_POINT ( 'NONE',  ( -68.57415822541635464, -18.01420295945611727, 95.00000000000000000 ) ) ;
#19883 = CARTESIAN_POINT ( 'NONE',  ( 157.9999999999997726, 244.0787500750700474, 45.00000000000000000 ) ) ;
#19884 = CARTESIAN_POINT ( 'NONE',  ( 79.99999999999994316, 80.00000000000001421, 100.0000000000000142 ) ) ;
#19885 = DIRECTION ( 'NONE',  ( -0.8916010070293383105, -0.4528218681383106015, 0.000000000000000000 ) ) ;
#19886 = ORIENTED_EDGE ( 'NONE', *, *, #22919, .F. ) ;
#19887 = DIRECTION ( 'NONE',  ( 1.000000000000000000, 0.000000000000000000, -0.000000000000000000 ) ) ;
#19888 = ORIENTED_EDGE ( 'NONE', *, *, #7646, .F. ) ;
#19889 = EDGE_CURVE ( 'NONE', #5660, #15498, #23282, .T. ) ;
#19890 = DIRECTION ( 'NONE',  ( 0.4528218681382319422, 0.8916010070293783896, -0.000000000000000000 ) ) ;
#19891 = CARTESIAN_POINT ( 'NONE',  ( -221.9128906662286340, 61.41899577391678378, -10.11264670733106463 ) ) ;
#19892 = CARTESIAN_POINT ( 'NONE',  ( 158.0000000000014211, 70.52749954957745615, -45.00000000000000000 ) ) ;
#19893 = VERTEX_POINT ( 'NONE', #25709 ) ;
#19894 = CARTESIAN_POINT ( 'NONE',  ( -260.0000000000001137, -170.0000000000001137, -59.99999999999986500 ) ) ;
#19895 = VERTEX_POINT ( 'NONE', #20840 ) ;
#19896 = TOROIDAL_SURFACE ( 'NONE', #6520, 11.00000000000001066, 1.000000000000000000 ) ;
#19897 = DIRECTION ( 'NONE',  ( -0.000000000000000000, -0.000000000000000000, -1.000000000000000000 ) ) ;
#19898 = ORIENTED_EDGE ( 'NONE', *, *, #27186, .F. ) ;
#19899 = DIRECTION ( 'NONE',  ( -0.000000000000000000, 0.000000000000000000, -1.000000000000000000 ) ) ;
#19900 = EDGE_LOOP ( 'NONE', ( #10048, #21455, #897, #12643 ) ) ;
#19901 = VECTOR ( 'NONE', #5543, 1000.000000000000000 ) ;
#19902 = ORIENTED_EDGE ( 'NONE', *, *, #10522, .T. ) ;
#19903 = EDGE_CURVE ( 'NONE', #9517, #1905, #3727, .T. ) ;
#19904 = DIRECTION ( 'NONE',  ( 0.8916010070296834789, -0.4528218681376312005, 0.000000000000000000 ) ) ;
#19905 = ADVANCED_FACE ( 'NONE', ( #7773 ), #21118, .F. ) ;
#19906 = ORIENTED_EDGE ( 'NONE', *, *, #1180, .F. ) ;
#19907 = ORIENTED_EDGE ( 'NONE', *, *, #15561, .T. ) ;
#19908 = CARTESIAN_POINT ( 'NONE',  ( -227.3657730843038109, 133.9833936510421211, 14.99191580167116733 ) ) ;
#19909 = CARTESIAN_POINT ( 'NONE',  ( 103.7569845406553668, 245.1294976011697884, 26.47883977338666739 ) ) ;
#19910 = CARTESIAN_POINT ( 'NONE',  ( 134.9999999999998579, 457.0747856552986832, -152.5098566583459672 ) ) ;
#19911 = DIRECTION ( 'NONE',  ( 0.000000000000000000, 0.000000000000000000, -1.000000000000000000 ) ) ;
#19912 = VECTOR ( 'NONE', #6726, 1000.000000000000000 ) ;
#19913 = ADVANCED_FACE ( 'NONE', ( #3448 ), #26253, .T. ) ;
#19914 = DIRECTION ( 'NONE',  ( 1.000000000000000000, 0.000000000000000000, 0.000000000000000000 ) ) ;
#19915 = FACE_OUTER_BOUND ( 'NONE', #10381, .T. ) ;
#19916 = CARTESIAN_POINT ( 'NONE',  ( -63.57415822541634043, 75.97823757117562593, 100.0000000000000000 ) ) ;
#19917 = DIRECTION ( 'NONE',  ( -0.000000000000000000, -0.000000000000000000, 1.000000000000000000 ) ) ;
#19918 = CARTESIAN_POINT ( 'NONE',  ( -275.9937304809269563, -170.0000000000001421, -91.21489442788019630 ) ) ;
#19919 = DIRECTION ( 'NONE',  ( -1.000000000000000000, 0.000000000000000000, 0.000000000000000000 ) ) ;
#19920 = CARTESIAN_POINT ( 'NONE',  ( 158.0000000000015064, 61.00387452705632541, 45.00000000000000000 ) ) ;
#19921 = CARTESIAN_POINT ( 'NONE',  ( 158.0000000000017337, 40.94087446699997912, -45.00000000000000000 ) ) ;
#19922 = EDGE_CURVE ( 'NONE', #17211, #26118, #1481, .T. ) ;
#19923 = ORIENTED_EDGE ( 'NONE', *, *, #2019, .F. ) ;
#19924 = CARTESIAN_POINT ( 'NONE',  ( 157.9999999999997726, 243.5708750675630370, 45.00000000000000000 ) ) ;
#19925 = EDGE_CURVE ( 'NONE', #25545, #6472, #17534, .T. ) ;
#19926 = CARTESIAN_POINT ( 'NONE',  ( 109.9999999999999147, 140.0000000000000000, 90.00000000000002842 ) ) ;
#19927 = PLANE ( 'NONE',  #7088 ) ;
#19928 = EDGE_CURVE ( 'NONE', #22920, #2445, #24884, .T. ) ;
#19929 = LINE ( 'NONE', #9017, #26665 ) ;
#19930 = ORIENTED_EDGE ( 'NONE', *, *, #12419, .F. ) ;
#19931 = FACE_OUTER_BOUND ( 'NONE', #6718, .T. ) ;
#19932 = VERTEX_POINT ( 'NONE', #10348 ) ;
#19933 = DIRECTION ( 'NONE',  ( 0.8916010070298360235, 0.4528218681373308296, 0.000000000000000000 ) ) ;
#19934 = ORIENTED_EDGE ( 'NONE', *, *, #16315, .F. ) ;
#19935 = CIRCLE ( 'NONE', #9853, 1.999999999999989564 ) ;
#19936 = ORIENTED_EDGE ( 'NONE', *, *, #5364, .F. ) ;
#19937 = ORIENTED_EDGE ( 'NONE', *, *, #8300, .F. ) ;
#19938 = EDGE_CURVE ( 'NONE', #7676, #2950, #16678, .T. ) ;
#19939 = EDGE_LOOP ( 'NONE', ( #27972, #6409, #3510, #16797 ) ) ;
#19940 = AXIS2_PLACEMENT_3D ( 'NONE', #16204, #255, #9452 ) ;
#19941 = ORIENTED_EDGE ( 'NONE', *, *, #804, .F. ) ;
#19942 = VERTEX_POINT ( 'NONE', #5753 ) ;
#19943 = LINE ( 'NONE', #15506, #21900 ) ;
#19944 = DIRECTION ( 'NONE',  ( -0.000000000000000000, -0.000000000000000000, -1.000000000000000000 ) ) ;
#19945 = CARTESIAN_POINT ( 'NONE',  ( 0.000000000000000000, 75.97823757117562593, 95.00000000000000000 ) ) ;
#19946 = CARTESIAN_POINT ( 'NONE',  ( -277.2150368962633706, -237.2150368962634559, -110.0000000000000284 ) ) ;
#19947 = CARTESIAN_POINT ( 'NONE',  ( -209.7310389751728508, 59.98715598645322444, 17.47553936828792587 ) ) ;
#19948 = DIRECTION ( 'NONE',  ( -9.251858538542974046E-17, -1.214306433183764966E-16, 1.000000000000000000 ) ) ;
#19949 = CARTESIAN_POINT ( 'NONE',  ( 367.4999999999996021, 44.41075299063186321, -100.0000000000000142 ) ) ;
#19950 = CARTESIAN_POINT ( 'NONE',  ( 187.4999999999996305, -5.589247009368157215, 74.99999999999995737 ) ) ;
#19951 = VECTOR ( 'NONE', #15338, 1000.000000000000000 ) ;
#19952 = LINE ( 'NONE', #26409, #17189 ) ;
#19953 = DIRECTION ( 'NONE',  ( -0.5000000000000039968, -0.8660254037844362651, -1.224646799147353454E-16 ) ) ;
#19954 = DIRECTION ( 'NONE',  ( 0.000000000000000000, 0.000000000000000000, 1.000000000000000000 ) ) ;
#19955 = AXIS2_PLACEMENT_3D ( 'NONE', #25009, #5325, #14101 ) ;
#19956 = EDGE_CURVE ( 'NONE', #14934, #20505, #3305, .T. ) ;
#19957 = EDGE_CURVE ( 'NONE', #4647, #12815, #17801, .T. ) ;
#19958 = CARTESIAN_POINT ( 'NONE',  ( -8.311916932730307295, 131.0476075684319994, 16.36633293656888810 ) ) ;
#19959 = PLANE ( 'NONE',  #18341 ) ;
#19960 = CARTESIAN_POINT ( 'NONE',  ( 157.4999999999998579, 100.8759371434154701, 45.00000000000000000 ) ) ;
#19961 = VECTOR ( 'NONE', #16445, 1000.000000000000114 ) ;
#19963 = ORIENTED_EDGE ( 'NONE', *, *, #12030, .T. ) ;
#19962 = ORIENTED_EDGE ( 'NONE', *, *, #24395, .F. ) ;
#19964 = CARTESIAN_POINT ( 'NONE',  ( -161.8971216350977329, 118.9700043538931737, 23.57800815686201190 ) ) ;
#19965 = DIRECTION ( 'NONE',  ( -0.000000000000000000, -0.000000000000000000, -1.000000000000000000 ) ) ;
#19966 = DIRECTION ( 'NONE',  ( 0.000000000000000000, -1.000000000000000000, 0.000000000000000000 ) ) ;
#19967 = ORIENTED_EDGE ( 'NONE', *, *, #28176, .F. ) ;
#19968 = CONTEXT_DEPENDENT_SHAPE_REPRESENTATION ( #26155, #6367 ) ;
#19969 = VERTEX_POINT ( 'NONE', #8908 ) ;
#19970 = VERTEX_POINT ( 'NONE', #15092 ) ;
#19971 = FACE_OUTER_BOUND ( 'NONE', #25374, .T. ) ;
#19972 = DIRECTION ( 'NONE',  ( -0.8916010070293584056, -0.4528218681382712996, 0.000000000000000000 ) ) ;
#19973 = ORIENTED_EDGE ( 'NONE', *, *, #8286, .F. ) ;
#19974 = ORIENTED_EDGE ( 'NONE', *, *, #400, .T. ) ;
#19975 = AXIS2_PLACEMENT_3D ( 'NONE', #3657, #4079, #14732 ) ;
#19976 = AXIS2_PLACEMENT_3D ( 'NONE', #1246, #19191, #16897 ) ;
#19977 = PLANE ( 'NONE',  #1253 ) ;
#19978 = CARTESIAN_POINT ( 'NONE',  ( -201.5823348103256478, 94.41654411267251135, -29.50230888136551854 ) ) ;
#19979 = ORIENTED_EDGE ( 'NONE', *, *, #16587, .T. ) ;
#19980 = CARTESIAN_POINT ( 'NONE',  ( -207.8757358334619312, 89.94749888897153767, 26.37785067087564883 ) ) ;
#19981 = CIRCLE ( 'NONE', #5743, 60.59270260175150469 ) ;
#19982 = CARTESIAN_POINT ( 'NONE',  ( 39.99999999999995737, 59.99999999999980105, 80.00000000000001421 ) ) ;
#19983 = CARTESIAN_POINT ( 'NONE',  ( 157.9999999999999432, 213.4763749774776045, -45.00000000000000000 ) ) ;
#19984 = CARTESIAN_POINT ( 'NONE',  ( 159.9611678081874402, 203.3574085914958118, -150.6837522856751264 ) ) ;
#19985 = ADVANCED_FACE ( 'NONE', ( #12800 ), #20758, .F. ) ;
#19986 = ORIENTED_EDGE ( 'NONE', *, *, #13349, .F. ) ;
#19987 = DIRECTION ( 'NONE',  ( 0.8916010070293384215, 0.4528218681383106015, 0.000000000000000000 ) ) ;
#19988 = EDGE_CURVE ( 'NONE', #7037, #26389, #4581, .T. ) ;
#19989 = AXIS2_PLACEMENT_3D ( 'NONE', #2559, #26407, #22107 ) ;
#19990 = CARTESIAN_POINT ( 'NONE',  ( 158.0000000000003411, 173.8582498648732440, -45.00000000000000000 ) ) ;
#19991 = DIRECTION ( 'NONE',  ( -1.000000000000000000, 0.000000000000000000, 0.000000000000000000 ) ) ;
#19992 = CARTESIAN_POINT ( 'NONE',  ( 158.0000000000009948, 108.6534996696901345, -45.00000000000000000 ) ) ;
#19993 = EDGE_LOOP ( 'NONE', ( #11836, #26042, #21547, #17706 ) ) ;
#19994 = AXIS2_PLACEMENT_3D ( 'NONE', #893, #9666, #18421 ) ;
#19995 = PLANE ( 'NONE',  #5458 ) ;
#19996 = DIRECTION ( 'NONE',  ( -0.9506505318133474658, 0.3102637045530776683, 0.000000000000000000 ) ) ;
#19997 = DIRECTION ( 'NONE',  ( -0.000000000000000000, 1.000000000000000000, -1.387778780781445429E-16 ) ) ;
#19998 = VERTEX_POINT ( 'NONE', #15385 ) ;
#19999 = VECTOR ( 'NONE', #16367, 1000.000000000000000 ) ;
#20000 = VERTEX_POINT ( 'NONE', #13367 ) ;
#20001 = CARTESIAN_POINT ( 'NONE',  ( 157.4999999999998579, 181.1279373836408411, 45.00000000000000000 ) ) ;
#20002 = CARTESIAN_POINT ( 'NONE',  ( -202.4550896089758112, 93.28604070817037552, -30.13616383332644588 ) ) ;
#20003 = ORIENTED_EDGE ( 'NONE', *, *, #15420, .T. ) ;
#20004 = VERTEX_POINT ( 'NONE', #13089 ) ;
#20005 = DIRECTION ( 'NONE',  ( 0.9961946980917455452, 0.000000000000000000, -0.08715574274765836016 ) ) ;
#20006 = CARTESIAN_POINT ( 'NONE',  ( 157.4999999999998579, 138.4940622560211239, 45.00000000000000000 ) ) ;
#20007 = ORIENTED_EDGE ( 'NONE', *, *, #23454, .F. ) ;
#20008 = EDGE_LOOP ( 'NONE', ( #7804, #26675, #22520, #18740 ) ) ;
#20009 = CIRCLE ( 'NONE', #27797, 22.49999999999999289 ) ;
#20010 = DIRECTION ( 'NONE',  ( -0.000000000000000000, 1.000000000000000000, -1.387778780781445429E-16 ) ) ;
#20011 = ADVANCED_FACE ( 'NONE', ( #24272 ), #10634, .F. ) ;
#20012 = DIRECTION ( 'NONE',  ( -0.000000000000000000, -0.000000000000000000, 1.000000000000000000 ) ) ;
#20013 = FACE_OUTER_BOUND ( 'NONE', #24195, .T. ) ;
#20014 = CARTESIAN_POINT ( 'NONE',  ( -8.492276074956963683, 132.4970898450557399, -14.40628465233269218 ) ) ;
#20015 = VECTOR ( 'NONE', #15624, 1000.000000000000114 ) ;
#20016 = CARTESIAN_POINT ( 'NONE',  ( -119.0030847931093518, 214.2064521616282775, 15.00000000000000000 ) ) ;
#20017 = DIRECTION ( 'NONE',  ( 0.4528218681378510801, -0.8916010070295719014, 0.000000000000000000 ) ) ;
#20018 = DIRECTION ( 'NONE',  ( 0.8916010070293283185, 0.4528218681383305855, 0.000000000000000000 ) ) ;
#20019 = ORIENTED_EDGE ( 'NONE', *, *, #12091, .F. ) ;
#20020 = CARTESIAN_POINT ( 'NONE',  ( -10.78991826960876033, 200.8449754580304898, -45.00000000000000000 ) ) ;
#20021 = ADVANCED_FACE ( 'NONE', ( #6313 ), #8480, .F. ) ;
#20022 = LINE ( 'NONE', #4642, #10629 ) ;
#20023 = CARTESIAN_POINT ( 'NONE',  ( 203.1730087600953993, 54.44004362106413453, 45.00000000000000000 ) ) ;
#20024 = DIRECTION ( 'NONE',  ( 1.000000000000000000, 0.000000000000000000, 0.000000000000000000 ) ) ;
#20025 = ORIENTED_EDGE ( 'NONE', *, *, #12034, .T. ) ;
#20026 = DIRECTION ( 'NONE',  ( 0.4528218681372909171, -0.8916010070298563406, 0.000000000000000000 ) ) ;
#20027 = VERTEX_POINT ( 'NONE', #21971 ) ;
#20028 = ADVANCED_FACE ( 'NONE', ( #4012 ), #12067, .T. ) ;
#20029 = DIRECTION ( 'NONE',  ( -0.000000000000000000, -0.000000000000000000, 1.000000000000000000 ) ) ;
#20030 = DIRECTION ( 'NONE',  ( -0.2066290158914539099, 0.9784193629480814058, 0.000000000000000000 ) ) ;
#20031 = FACE_OUTER_BOUND ( 'NONE', #10515, .T. ) ;
#20032 = VERTEX_POINT ( 'NONE', #28140 ) ;
#20033 = LINE ( 'NONE', #15747, #23050 ) ;
#20034 = VERTEX_POINT ( 'NONE', #21839 ) ;
#20035 = AXIS2_PLACEMENT_3D ( 'NONE', #18601, #27351, #7267 ) ;
#20036 = DIRECTION ( 'NONE',  ( 0.000000000000000000, -1.000000000000000000, 0.000000000000000000 ) ) ;
#20037 = VERTEX_POINT ( 'NONE', #22116 ) ;
#20038 = DIRECTION ( 'NONE',  ( -0.8916010070293711731, 0.4528218681382463751, 0.000000000000000000 ) ) ;
#20039 = VERTEX_POINT ( 'NONE', #1856 ) ;
#20040 = ADVANCED_FACE ( 'NONE', ( #10918 ), #27196, .T. ) ;
#20041 = ORIENTED_EDGE ( 'NONE', *, *, #11827, .F. ) ;
#20042 = DIRECTION ( 'NONE',  ( 0.000000000000000000, 0.000000000000000000, -1.000000000000000000 ) ) ;
#20043 = ORIENTED_EDGE ( 'NONE', *, *, #3085, .F. ) ;
#20044 = ORIENTED_EDGE ( 'NONE', *, *, #12561, .F. ) ;
#20045 = VERTEX_POINT ( 'NONE', #9048 ) ;
#20046 = CARTESIAN_POINT ( 'NONE',  ( 88.62124187924879948, 239.8086506234586750, 16.24979138471424989 ) ) ;
#20047 = EDGE_CURVE ( 'NONE', #27897, #7159, #17515, .T. ) ;
#20048 = LINE ( 'NONE', #381, #19951 ) ;
#20049 = CARTESIAN_POINT ( 'NONE',  ( 217.4999999999996305, 133.0668745871126930, -30.86484227207697018 ) ) ;
#20050 = VECTOR ( 'NONE', #13672, 1000.000000000000000 ) ;
#20051 = CLOSED_SHELL ( 'NONE', ( #21834, #1810, #14290, #173, #11742, #9565, #6818, #3931, #19662, #27565, #473, #7023, #2634, #4503, #1993, #23028, #26539, #7933, #13948, #13171, #2566, #2494, #18885, #12619, #539, #7293, #2453, #4594, #22398, #5775, #17523, #19913, #10612, #13393, #3995, #4546, #15944, #28010, #18522, #8665, #21088, #19584 ) ) ;
#20052 = DIRECTION ( 'NONE',  ( 0.000000000000000000, -1.000000000000000000, 0.000000000000000000 ) ) ;
#20053 = DIRECTION ( 'NONE',  ( 0.000000000000000000, 0.000000000000000000, 1.000000000000000000 ) ) ;
#20054 = CARTESIAN_POINT ( 'NONE',  ( 9.999999999999964473, 60.00000000000001421, 110.0000000000000284 ) ) ;
#20055 = CARTESIAN_POINT ( 'NONE',  ( 158.0000000000008811, 123.1928747072253572, -45.00000000000000000 ) ) ;
#20056 = CARTESIAN_POINT ( 'NONE',  ( -58.76345596729049703, 58.76345596729049703, -45.00000000000000000 ) ) ;
#20057 = CARTESIAN_POINT ( 'NONE',  ( -37.82257053376181233, 71.03850157808263077, 100.0000000000000000 ) ) ;
#20058 = DIRECTION ( 'NONE',  ( 1.000000000000000000, 0.000000000000000000, 0.000000000000000000 ) ) ;
#20059 = LINE ( 'NONE', #13762, #11644 ) ;
#20060 = ORIENTED_EDGE ( 'NONE', *, *, #18434, .T. ) ;
#20061 = CARTESIAN_POINT ( 'NONE',  ( 157.4999999999998010, 233.7933125412885147, 45.00000000000000000 ) ) ;
#20062 = EDGE_CURVE ( 'NONE', #10685, #5551, #11150, .T. ) ;
#20063 = EDGE_CURVE ( 'NONE', #25077, #28289, #21683, .T. ) ;
#20064 = LINE ( 'NONE', #396, #16074 ) ;
#20065 = LINE ( 'NONE', #22084, #27277 ) ;
#20066 = CARTESIAN_POINT ( 'NONE',  ( 0.03738397811494300477, -1.250000000000000666, 7.196583346711943108 ) ) ;
#20067 = ORIENTED_EDGE ( 'NONE', *, *, #26151, .T. ) ;
#20068 = AXIS2_PLACEMENT_3D ( 'NONE', #5642, #21002, #3901 ) ;
#20069 = CARTESIAN_POINT ( 'NONE',  ( -112.3221550338875687, 74.54464929955099706, 83.00000000000001421 ) ) ;
#20070 = ORIENTED_EDGE ( 'NONE', *, *, #15206, .T. ) ;
#20071 = VERTEX_POINT ( 'NONE', #8624 ) ;
#20072 = AXIS2_PLACEMENT_3D ( 'NONE', #22845, #10904, #6587 ) ;
#20073 = EDGE_CURVE ( 'NONE', #23817, #11039, #143, .T. ) ;
#20074 = ORIENTED_EDGE ( 'NONE', *, *, #21247, .T. ) ;
#20075 = VECTOR ( 'NONE', #17188, 1000.000000000000000 ) ;
#20076 = ADVANCED_FACE ( 'NONE', ( #26137 ), #6461, .F. ) ;
#20077 = ORIENTED_EDGE ( 'NONE', *, *, #9389, .T. ) ;
#20078 = ORIENTED_EDGE ( 'NONE', *, *, #26079, .F. ) ;
#20079 = EDGE_LOOP ( 'NONE', ( #20365, #23017, #26719, #25867 ) ) ;
#20080 = FACE_OUTER_BOUND ( 'NONE', #19580, .T. ) ;
#20081 = LINE ( 'NONE', #2407, #22837 ) ;
#20082 = CARTESIAN_POINT ( 'NONE',  ( -51.90955279280624524, 193.7290884209386661, 45.00000000000000000 ) ) ;
#20083 = CARTESIAN_POINT ( 'NONE',  ( 157.4999999999998579, 43.19481197075347723, -45.00000000000000000 ) ) ;
#20084 = EDGE_CURVE ( 'NONE', #13314, #9427, #2283, .T. ) ;
#20085 = PRODUCT_DEFINITION_CONTEXT ( 'detailed design', #8551, 'design' ) ;
#20086 = LINE ( 'NONE', #24835, #28142 ) ;
#20087 = CARTESIAN_POINT ( 'NONE',  ( -222.4720504096164007, 61.14635810690615614, 21.27434031932121172 ) ) ;
#20089 = DIRECTION ( 'NONE',  ( -0.000000000000000000, -0.000000000000000000, -1.000000000000000000 ) ) ;
#20088 = VECTOR ( 'NONE', #21965, 1000.000000000000000 ) ;
#20090 = DIRECTION ( 'NONE',  ( -0.000000000000000000, -0.000000000000000000, -1.000000000000000000 ) ) ;
#20091 = CARTESIAN_POINT ( 'NONE',  ( 217.4999999999996589, 194.4107529906318064, 100.0000000000000284 ) ) ;
#20092 = CIRCLE ( 'NONE', #4026, 5.999999999999991118 ) ;
#20093 = LINE ( 'NONE', #15378, #21787 ) ;
#20094 = CARTESIAN_POINT ( 'NONE',  ( 157.4999999999998010, 233.7933125412885147, 45.00000000000000000 ) ) ;
#20095 = LINE ( 'NONE', #3130, #13216 ) ;
#20096 = FACE_BOUND ( 'NONE', #9684, .T. ) ;
#20097 = CARTESIAN_POINT ( 'NONE',  ( -4.127814339125048804, 134.2316681395303988, 15.51991914718412779 ) ) ;
#20098 = DIRECTION ( 'NONE',  ( 0.000000000000000000, 0.000000000000000000, 1.000000000000000000 ) ) ;
#20099 = DIRECTION ( 'NONE',  ( 0.8916010070295817824, -0.4528218681378317623, 0.000000000000000000 ) ) ;
#20100 = LINE ( 'NONE', #433, #6092 ) ;
#20102 = ORIENTED_EDGE ( 'NONE', *, *, #11520, .T. ) ;
#20101 = ORIENTED_EDGE ( 'NONE', *, *, #25586, .F. ) ;
#20103 = CARTESIAN_POINT ( 'NONE',  ( 158.0000000000015632, 57.98812451204224061, 45.00000000000000000 ) ) ;
#20104 = AXIS2_PLACEMENT_3D ( 'NONE', #26527, #9023, #4695 ) ;
#20105 = CARTESIAN_POINT ( 'NONE',  ( 157.9999999999998295, 226.0157500150140208, -45.00000000000000000 ) ) ;
#20106 = LINE ( 'NONE', #21843, #1175 ) ;
#20107 = VERTEX_POINT ( 'NONE', #15525 ) ;
#20108 = CONTEXT_DEPENDENT_SHAPE_REPRESENTATION ( #8922, #6140 ) ;
#20109 = ORIENTED_EDGE ( 'NONE', *, *, #22259, .F. ) ;
#20110 = ORIENTED_EDGE ( 'NONE', *, *, #26768, .T. ) ;
#20111 = AXIS2_PLACEMENT_3D ( 'NONE', #4828, #17763, #682 ) ;
#20112 = DIRECTION ( 'NONE',  ( -0.8916010070293682865, -0.4528218681382519262, 0.000000000000000000 ) ) ;
#20113 = DIRECTION ( 'NONE',  ( 0.000000000000000000, 0.000000000000000000, -1.000000000000000000 ) ) ;
#20114 = AXIS2_PLACEMENT_3D ( 'NONE', #20162, #13284, #2198 ) ;
#20115 = ORIENTED_EDGE ( 'NONE', *, *, #14390, .T. ) ;
#20116 = ORIENTED_EDGE ( 'NONE', *, *, #18687, .F. ) ;
#20117 = DIRECTION ( 'NONE',  ( 0.4528218681372122578, 0.8916010070298964196, -0.000000000000000000 ) ) ;
#20118 = EDGE_CURVE ( 'NONE', #905, #3644, #24847, .T. ) ;
#20119 = LINE ( 'NONE', #19836, #10057 ) ;
#20120 = VERTEX_POINT ( 'NONE', #9487 ) ;
#20121 = CARTESIAN_POINT ( 'NONE',  ( -206.1571879782320309, 90.87865330178034640, 27.62915181265775644 ) ) ;
#20122 = CARTESIAN_POINT ( 'NONE',  ( 158.0000000000012790, 85.57474959461971764, 45.00000000000000000 ) ) ;
#20123 = VECTOR ( 'NONE', #4898, 1000.000000000000000 ) ;
#20124 = DIRECTION ( 'NONE',  ( -0.000000000000000000, -0.000000000000000000, 1.000000000000000000 ) ) ;
#20125 = DIRECTION ( 'NONE',  ( 0.000000000000000000, 1.000000000000000000, 0.000000000000000000 ) ) ;
#20126 = CARTESIAN_POINT ( 'NONE',  ( -217.4092282431682577, 59.59925738963638508, -26.62835594396155869 ) ) ;
#20127 = ORIENTED_EDGE ( 'NONE', *, *, #4707, .T. ) ;
#20128 = DIRECTION ( 'NONE',  ( 1.000000000000000000, 8.673617379884036705E-17, -0.000000000000000000 ) ) ;
#20129 = AXIS2_PLACEMENT_3D ( 'NONE', #2740, #3159, #1011 ) ;
#20130 = LINE ( 'NONE', #19990, #12461 ) ;
#20131 = DIRECTION ( 'NONE',  ( -1.224646799147353207E-16, 1.000000000000000000, 0.000000000000000000 ) ) ;
#20132 = CARTESIAN_POINT ( 'NONE',  ( -17.24491960465745777, 0.000000000000000000, 100.0000000000000000 ) ) ;
#20133 = ORIENTED_EDGE ( 'NONE', *, *, #9537, .F. ) ;
#20134 = DIRECTION ( 'NONE',  ( 0.000000000000000000, 0.000000000000000000, -1.000000000000000000 ) ) ;
#20135 = CIRCLE ( 'NONE', #7761, 6.025000000000002132 ) ;
#20136 = EDGE_CURVE ( 'NONE', #6606, #23450, #20245, .T. ) ;
#20137 = LINE ( 'NONE', #468, #10269 ) ;
#20138 = DIRECTION ( 'NONE',  ( -0.000000000000000000, -0.000000000000000000, -1.000000000000000000 ) ) ;
#20139 = ORIENTED_EDGE ( 'NONE', *, *, #26721, .T. ) ;
#20140 = DIRECTION ( 'NONE',  ( 1.000000000000000000, 0.000000000000000000, 0.000000000000000000 ) ) ;
#20141 = ORIENTED_EDGE ( 'NONE', *, *, #21657, .F. ) ;
#20142 = DIRECTION ( 'NONE',  ( 0.000000000000000000, -1.000000000000000000, 0.000000000000000000 ) ) ;
#20143 = VECTOR ( 'NONE', #13582, 999.9999999999998863 ) ;
#20144 = CARTESIAN_POINT ( 'NONE',  ( -201.6498696902538939, 93.99348885415903965, -30.47085302539461438 ) ) ;
#20145 = ORIENTED_EDGE ( 'NONE', *, *, #7378, .F. ) ;
#20146 = MECHANICAL_DESIGN_GEOMETRIC_PRESENTATION_REPRESENTATION (  '', ( #2715 ), #7324 ) ;
#20147 = EDGE_CURVE ( 'NONE', #506, #8492, #18242, .T. ) ;
#20148 = ORIENTED_EDGE ( 'NONE', *, *, #25566, .T. ) ;
#20149 = EDGE_CURVE ( 'NONE', #19942, #9066, #11792, .T. ) ;
#20150 = CARTESIAN_POINT ( 'NONE',  ( 294.9233831825460470, 127.6681916698403398, -145.0000000000000000 ) ) ;
#20151 = EDGE_CURVE ( 'NONE', #10576, #19932, #13657, .T. ) ;
#20152 = VECTOR ( 'NONE', #718, 1000.000000000000114 ) ;
#20153 = PLANE ( 'NONE',  #27674 ) ;
#20154 = ADVANCED_FACE ( 'NONE', ( #854 ), #11505, .F. ) ;
#20155 = ORIENTED_EDGE ( 'NONE', *, *, #14592, .F. ) ;
#20156 = PLANE ( 'NONE',  #4557 ) ;
#20157 = ORIENTED_EDGE ( 'NONE', *, *, #21537, .F. ) ;
#20158 = CARTESIAN_POINT ( 'NONE',  ( 137.6105238444012286, 200.1711027725236534, -45.00000000000000000 ) ) ;
#20159 = DIRECTION ( 'NONE',  ( 0.000000000000000000, 0.5150380749100555988, 0.8571673007021114454 ) ) ;
#20160 = CARTESIAN_POINT ( 'NONE',  ( 157.4999999999998579, 100.8759371434154701, 45.00000000000000000 ) ) ;
#20161 = CARTESIAN_POINT ( 'NONE',  ( -33.82412182304897641, 129.4067652227780343, -16.89984886922910334 ) ) ;
#20162 = CARTESIAN_POINT ( 'NONE',  ( 134.9999999999998579, 220.0000000000000284, 45.00000000000000000 ) ) ;
#20163 = DIRECTION ( 'NONE',  ( 0.000000000000000000, 0.000000000000000000, 1.000000000000000000 ) ) ;
#20164 = CARTESIAN_POINT ( 'NONE',  ( 161.8967505429097287, 206.7072948235298782, -139.3076717160242595 ) ) ;
#20165 = ORIENTED_EDGE ( 'NONE', *, *, #15619, .F. ) ;
#20166 = CIRCLE ( 'NONE', #7783, 53.86582179324592090 ) ;
#20167 = DIRECTION ( 'NONE',  ( 0.8916010070293384215, 0.4528218681383106015, 0.000000000000000000 ) ) ;
#20168 = DIRECTION ( 'NONE',  ( 0.8916010070293384215, 0.4528218681383106015, 0.000000000000000000 ) ) ;
#20169 = LINE ( 'NONE', #210, #19206 ) ;
#20170 = CARTESIAN_POINT ( 'NONE',  ( -40.40953891503691153, 71.03850157808263077, 99.00000000000000000 ) ) ;
#20171 = ORIENTED_EDGE ( 'NONE', *, *, #13712, .F. ) ;
#20172 = CARTESIAN_POINT ( 'NONE',  ( -210.0000000000000284, 59.99999999999994316, 17.29233506344265336 ) ) ;
#20173 = VECTOR ( 'NONE', #18352, 1000.000000000000000 ) ;
#20174 = ORIENTED_EDGE ( 'NONE', *, *, #6271, .T. ) ;
#20175 = DIRECTION ( 'NONE',  ( 0.000000000000000000, 0.000000000000000000, 1.000000000000000000 ) ) ;
#20176 = DIRECTION ( 'NONE',  ( 1.000000000000000000, 0.000000000000000000, 0.000000000000000000 ) ) ;
#20177 = CARTESIAN_POINT ( 'NONE',  ( 138.0067716801852669, 249.8494523599397894, -139.8040206391607967 ) ) ;
#20178 = VERTEX_POINT ( 'NONE', #9340 ) ;
#20179 = CARTESIAN_POINT ( 'NONE',  ( -43.04748092857122543, 38.65804596583237895, 45.00000000000000000 ) ) ;
#20180 = DIRECTION ( 'NONE',  ( -0.5555587585212703461, -0.8314772792026879911, 1.901657040880024000E-15 ) ) ;
#20181 = ORIENTED_EDGE ( 'NONE', *, *, #34, .F. ) ;
#20182 = EDGE_CURVE ( 'NONE', #6540, #5518, #5013, .T. ) ;
#20183 = ADVANCED_FACE ( 'NONE', ( #9195 ), #720, .F. ) ;
#20184 = CARTESIAN_POINT ( 'NONE',  ( -227.3172910872899024, 73.27388443547883412, 17.24020071796984155 ) ) ;
#20185 = EDGE_LOOP ( 'NONE', ( #2435, #14781, #24966, #9913 ) ) ;
#20186 = DIRECTION ( 'NONE',  ( 0.4528218681379503896, -0.8916010070295214973, 0.000000000000000000 ) ) ;
#20187 = ORIENTED_EDGE ( 'NONE', *, *, #5112, .F. ) ;
#20188 = ORIENTED_EDGE ( 'NONE', *, *, #20807, .F. ) ;
#20189 = DIRECTION ( 'NONE',  ( 1.000000000000000000, 0.000000000000000000, 0.000000000000000000 ) ) ;
#20190 = ORIENTED_EDGE ( 'NONE', *, *, #12231, .F. ) ;
#20191 = VECTOR ( 'NONE', #18928, 1000.000000000000000 ) ;
#20192 = EDGE_CURVE ( 'NONE', #25123, #23090, #18493, .T. ) ;
#20193 = ORIENTED_EDGE ( 'NONE', *, *, #18053, .T. ) ;
#20194 = ORIENTED_EDGE ( 'NONE', *, *, #25406, .F. ) ;
#20195 = CARTESIAN_POINT ( 'NONE',  ( 91.45931183162105071, 239.6823639898985050, 17.19464119471847852 ) ) ;
#20196 = VECTOR ( 'NONE', #27616, 1000.000000000000114 ) ;
#20197 = EDGE_CURVE ( 'NONE', #13479, #4776, #16098, .T. ) ;
#20198 = CARTESIAN_POINT ( 'NONE',  ( 158.0000000000000568, 201.4448749474510407, -45.00000000000000000 ) ) ;
#20199 = CARTESIAN_POINT ( 'NONE',  ( 158.0000000000008242, 126.2086247222394206, 45.00000000000000000 ) ) ;
#20200 = DIRECTION ( 'NONE',  ( 0.7343588774761952154, -0.6787614006938686995, 0.000000000000000000 ) ) ;
#20201 = CARTESIAN_POINT ( 'NONE',  ( -305.0000000000001137, -165.0000000000001137, -110.0000000000000284 ) ) ;
#20202 = FACE_OUTER_BOUND ( 'NONE', #15749, .T. ) ;
#20203 = CARTESIAN_POINT ( 'NONE',  ( 112.4999999999998863, 220.0000000000000284, -105.0000000000000284 ) ) ;
#20204 = DIRECTION ( 'NONE',  ( 0.000000000000000000, -1.000000000000000000, 0.000000000000000000 ) ) ;
#20205 = DIRECTION ( 'NONE',  ( 0.8916010070293384215, 0.4528218681383106015, 0.000000000000000000 ) ) ;
#20206 = LINE ( 'NONE', #2673, #16456 ) ;
#20207 = DIRECTION ( 'NONE',  ( -1.000000000000000000, 0.000000000000000000, -0.000000000000000000 ) ) ;
#20208 = EDGE_LOOP ( 'NONE', ( #24203, #8805, #9802, #11472, #20251 ) ) ;
#20209 = LINE ( 'NONE', #25466, #26618 ) ;
#20210 = VECTOR ( 'NONE', #3655, 1000.000000000000000 ) ;
#20211 = DIRECTION ( 'NONE',  ( 0.8916010070295820045, -0.4528218681378310406, 0.000000000000000000 ) ) ;
#20212 = FACE_OUTER_BOUND ( 'NONE', #5977, .T. ) ;
#20213 = DIRECTION ( 'NONE',  ( 0.000000000000000000, 0.000000000000000000, 1.000000000000000000 ) ) ;
#20214 = ORIENTED_EDGE ( 'NONE', *, *, #18354, .F. ) ;
#20215 = AXIS2_PLACEMENT_3D ( 'NONE', #14699, #9299, #27749 ) ;
#20216 = EDGE_CURVE ( 'NONE', #20740, #9697, #13951, .T. ) ;
#20217 = PLANE ( 'NONE',  #11604 ) ;
#20218 = ORIENTED_EDGE ( 'NONE', *, *, #25163, .T. ) ;
#20219 = VERTEX_POINT ( 'NONE', #3000 ) ;
#20220 = ORIENTED_EDGE ( 'NONE', *, *, #1308, .T. ) ;
#20221 = ORIENTED_EDGE ( 'NONE', *, *, #27086, .F. ) ;
#20222 = ORIENTED_EDGE ( 'NONE', *, *, #12953, .F. ) ;
#20223 = CARTESIAN_POINT ( 'NONE',  ( -113.0087222755475267, 134.5426160695832607, 13.86259311301067854 ) ) ;
#20224 = DIRECTION ( 'NONE',  ( 0.000000000000000000, 0.000000000000000000, 1.000000000000000000 ) ) ;
#20225 = CARTESIAN_POINT ( 'NONE',  ( 158.0000000000004832, 163.3188748273380213, 45.00000000000000000 ) ) ;
#20226 = ADVANCED_FACE ( 'NONE', ( #18525 ), #22405, .F. ) ;
#20227 = VECTOR ( 'NONE', #23171, 1000.000000000000000 ) ;
#20228 = ADVANCED_FACE ( 'NONE', ( #20669 ), #12529, .F. ) ;
#20229 = DIRECTION ( 'NONE',  ( -1.000000000000000000, 0.000000000000000000, -0.000000000000000000 ) ) ;
#20230 = LINE ( 'NONE', #4854, #18546 ) ;
#20231 = AXIS2_PLACEMENT_3D ( 'NONE', #11816, #9652, #18548 ) ;
#20232 = CARTESIAN_POINT ( 'NONE',  ( -218.1276041038539972, 59.80742093790405534, 25.66002785713338952 ) ) ;
#20233 = DIRECTION ( 'NONE',  ( 0.000000000000000000, -0.000000000000000000, 1.000000000000000000 ) ) ;
#20234 = CARTESIAN_POINT ( 'NONE',  ( 184.7759657584203694, 39.02219989801907474, 45.00000000000000000 ) ) ;
#20235 = DIRECTION ( 'NONE',  ( 0.000000000000000000, 0.000000000000000000, -1.000000000000000000 ) ) ;
#20236 = DIRECTION ( 'NONE',  ( 0.8916010070298759915, -0.4528218681372521703, 0.000000000000000000 ) ) ;
#20237 = DIRECTION ( 'NONE',  ( -0.8916010070294801970, 0.4528218681380314914, 0.000000000000000000 ) ) ;
#20238 = CARTESIAN_POINT ( 'NONE',  ( 132.3894761555988282, 239.8288972274758919, -45.00000000000000000 ) ) ;
#20239 = CARTESIAN_POINT ( 'NONE',  ( 96.92716526683047107, 115.1868982021512124, 77.49999999971905140 ) ) ;
#20240 = EDGE_CURVE ( 'NONE', #28220, #2342, #24453, .T. ) ;
#20241 = ADVANCED_FACE ( 'NONE', ( #24414 ), #27269, .F. ) ;
#20242 = FACE_OUTER_BOUND ( 'NONE', #20008, .T. ) ;
#20243 = DIRECTION ( 'NONE',  ( 1.000000000000000000, 2.602085213965211135E-16, 0.000000000000000000 ) ) ;
#20244 = CARTESIAN_POINT ( 'NONE',  ( 203.1730087600953993, 54.44004362106413453, -45.00000000000000000 ) ) ;
#20245 = LINE ( 'NONE', #2861, #2880 ) ;
#20247 = ORIENTED_EDGE ( 'NONE', *, *, #12288, .F. ) ;
#20246 = ORIENTED_EDGE ( 'NONE', *, *, #17154, .T. ) ;
#20248 = CARTESIAN_POINT ( 'NONE',  ( 158.0000000000004547, 163.8267498348450886, 45.00000000000000000 ) ) ;
#20249 = CIRCLE ( 'NONE', #7443, 2.000000000000004885 ) ;
#20250 = FACE_OUTER_BOUND ( 'NONE', #14792, .T. ) ;
#20251 = ORIENTED_EDGE ( 'NONE', *, *, #19271, .F. ) ;
#20252 = EDGE_LOOP ( 'NONE', ( #13446, #545, #6706, #9350, #17665, #6443 ) ) ;
#20253 = AXIS2_PLACEMENT_3D ( 'NONE', #7681, #5374, #8099 ) ;
#20254 = VERTEX_POINT ( 'NONE', #9766 ) ;
#20255 = AXIS2_PLACEMENT_3D ( 'NONE', #16651, #16376, #3133 ) ;
#20256 = CYLINDRICAL_SURFACE ( 'NONE', #16632, 5.000000000000004441 ) ;
#20257 = CARTESIAN_POINT ( 'NONE',  ( -157.8382221595611270, 120.6940372157653485, 22.00304971980720481 ) ) ;
#20258 = ORIENTED_EDGE ( 'NONE', *, *, #27218, .T. ) ;
#20259 = ORIENTED_EDGE ( 'NONE', *, *, #18144, .T. ) ;
#20260 = DIRECTION ( 'NONE',  ( 0.000000000000000000, 0.000000000000000000, -1.000000000000000000 ) ) ;
#20261 = FACE_OUTER_BOUND ( 'NONE', #24855, .T. ) ;
#20262 = EDGE_CURVE ( 'NONE', #12360, #3882, #20100, .T. ) ;
#20263 = EDGE_CURVE ( 'NONE', #5588, #20045, #25822, .T. ) ;
#20264 = CARTESIAN_POINT ( 'NONE',  ( 217.4999999999996305, 258.6181251126050711, 1.387778780781445676E-14 ) ) ;
#20265 = ORIENTED_EDGE ( 'NONE', *, *, #16188, .T. ) ;
#20266 = CARTESIAN_POINT ( 'NONE',  ( 158.0000000000013358, 80.55899957960563995, -45.00000000000000000 ) ) ;
#20267 = LINE ( 'NONE', #22715, #17124 ) ;
#20268 = VECTOR ( 'NONE', #26473, 1000.000000000000000 ) ;
#20269 = DIRECTION ( 'NONE',  ( 0.4528218681372509491, -0.8916010070298766577, 0.000000000000000000 ) ) ;
#20270 = VECTOR ( 'NONE', #7649, 1000.000000000000114 ) ;
#20271 = CARTESIAN_POINT ( 'NONE',  ( 158.0000000000015632, 57.98812451204224061, -45.00000000000000000 ) ) ;
#20272 =( GEOMETRIC_REPRESENTATION_CONTEXT ( 3 ) GLOBAL_UNCERTAINTY_ASSIGNED_CONTEXT ( ( #4566 ) ) GLOBAL_UNIT_ASSIGNED_CONTEXT ( ( #22156, #22590, #24601 ) ) REPRESENTATION_CONTEXT ( 'NONE', 'WORKASPACE' ) );
#20273 = CARTESIAN_POINT ( 'NONE',  ( -216.4559255058941289, 59.30400871604184232, -28.11406665935971461 ) ) ;
#20274 = MECHANICAL_DESIGN_GEOMETRIC_PRESENTATION_REPRESENTATION (  '', ( #95 ), #16616 ) ;
#20275 = VERTEX_POINT ( 'NONE', #5438 ) ;
#20276 = DIRECTION ( 'NONE',  ( 0.8916010070295410372, -0.4528218681379115873, 0.000000000000000000 ) ) ;
#20277 = CARTESIAN_POINT ( 'NONE',  ( -216.4421519707229891, 141.6000904446840707, -15.00000000000000178 ) ) ;
#20278 = LINE ( 'NONE', #463, #1923 ) ;
#20279 = CARTESIAN_POINT ( 'NONE',  ( -140.1213116003368668, 122.5384136796733827, -13.00000000000000000 ) ) ;
#20280 = ORIENTED_EDGE ( 'NONE', *, *, #5164, .T. ) ;
#20281 = EDGE_CURVE ( 'NONE', #26421, #23616, #19468, .T. ) ;
#20282 = CARTESIAN_POINT ( 'NONE',  ( -123.8208147886770121, 198.8605305197760913, 12.99999999999999822 ) ) ;
#20283 = EDGE_CURVE ( 'NONE', #7328, #21528, #13453, .T. ) ;
#20284 = CARTESIAN_POINT ( 'NONE',  ( -254.3350114625770289, -91.18033988749901653, 16.36034929305424512 ) ) ;
#20285 = DIRECTION ( 'NONE',  ( 0.000000000000000000, 0.000000000000000000, -1.000000000000000000 ) ) ;
#20286 = ORIENTED_EDGE ( 'NONE', *, *, #7063, .F. ) ;
#20287 = EDGE_CURVE ( 'NONE', #25781, #5376, #1791, .T. ) ;
#20288 = EDGE_LOOP ( 'NONE', ( #21015, #19967, #20007, #10547 ) ) ;
#20289 = CARTESIAN_POINT ( 'NONE',  ( 101.7779539749746931, 119.2876405404125393, 82.50000000030260594 ) ) ;
#20290 = PLANE ( 'NONE',  #17697 ) ;
#20291 = ORIENTED_EDGE ( 'NONE', *, *, #2082, .T. ) ;
#20292 = AXIS2_PLACEMENT_3D ( 'NONE', #2016, #15678, #13522 ) ;
#20293 = ORIENTED_EDGE ( 'NONE', *, *, #14715, .T. ) ;
#20294 = CARTESIAN_POINT ( 'NONE',  ( -141.6428522700808230, 69.54464929955099706, 83.00000000000001421 ) ) ;
#20295 = VECTOR ( 'NONE', #15821, 1000.000000000000000 ) ;
#20296 = DIRECTION ( 'NONE',  ( 1.000000000000000000, 0.000000000000000000, 0.000000000000000000 ) ) ;
#20297 = EDGE_LOOP ( 'NONE', ( #903, #10925 ) ) ;
#20298 = CARTESIAN_POINT ( 'NONE',  ( -205.1370039499190625, 144.1304017549904586, 12.99999999999999822 ) ) ;
#20299 = ORIENTED_EDGE ( 'NONE', *, *, #600, .T. ) ;
#20300 = CARTESIAN_POINT ( 'NONE',  ( 157.9999999999998010, 231.5393750375350237, 45.00000000000000000 ) ) ;
#20301 = FACE_OUTER_BOUND ( 'NONE', #9705, .T. ) ;
#20302 = CARTESIAN_POINT ( 'NONE',  ( -5.209541383816244320, 133.7633409757595757, -15.61671784922240214 ) ) ;
#20303 = CARTESIAN_POINT ( 'NONE',  ( -175.0000000000000000, -120.0250000000001904, -69.99999999999998579 ) ) ;
#20304 = VECTOR ( 'NONE', #22681, 1000.000000000000000 ) ;
#20305 = CARTESIAN_POINT ( 'NONE',  ( 158.0000000000004263, 168.3346248423521274, 45.00000000000000000 ) ) ;
#20306 = CARTESIAN_POINT ( 'NONE',  ( 160.9807621135329612, 204.9999999999999147, -138.9999999999999432 ) ) ;
#20307 = ORIENTED_EDGE ( 'NONE', *, *, #1286, .T. ) ;
#20308 = AXIS2_PLACEMENT_3D ( 'NONE', #21769, #8273, #23779 ) ;
#20309 = CARTESIAN_POINT ( 'NONE',  ( 282.4999999999996589, 19.41075299063184900, 80.49671038392669686 ) ) ;
#20310 = EDGE_CURVE ( 'NONE', #22340, #25311, #1055, .T. ) ;
#20311 = DIRECTION ( 'NONE',  ( -4.625929269271489858E-16, 0.000000000000000000, -1.000000000000000000 ) ) ;
#20312 = CARTESIAN_POINT ( 'NONE',  ( 158.0000000000003126, 178.3661248723802828, 45.00000000000000000 ) ) ;
#20313 = LINE ( 'NONE', #15737, #16688 ) ;
#20314 = ORIENTED_EDGE ( 'NONE', *, *, #19066, .T. ) ;
#20315 = DIRECTION ( 'NONE',  ( -0.3102637045530683979, 0.9506505318133506854, 0.000000000000000000 ) ) ;
#20316 = VECTOR ( 'NONE', #20036, 1000.000000000000000 ) ;
#20317 = EDGE_CURVE ( 'NONE', #23684, #7444, #1947, .T. ) ;
#20318 = ORIENTED_EDGE ( 'NONE', *, *, #27526, .F. ) ;
#20319 = EDGE_CURVE ( 'NONE', #17958, #9931, #5622, .T. ) ;
#20320 = DIRECTION ( 'NONE',  ( 0.000000000000000000, 0.000000000000000000, -1.000000000000000000 ) ) ;
#20321 = DIRECTION ( 'NONE',  ( 0.000000000000000000, 0.000000000000000000, 1.000000000000000000 ) ) ;
#20322 = DIRECTION ( 'NONE',  ( 0.000000000000000000, -0.000000000000000000, -1.000000000000000000 ) ) ;
#20323 = ORIENTED_EDGE ( 'NONE', *, *, #16092, .T. ) ;
#20324 = CARTESIAN_POINT ( 'NONE',  ( -260.0000000000001137, -152.0000000000000284, 60.00000000000002132 ) ) ;
#20325 = FACE_OUTER_BOUND ( 'NONE', #888, .T. ) ;
#20326 = ORIENTED_EDGE ( 'NONE', *, *, #3475, .F. ) ;
#20327 = CARTESIAN_POINT ( 'NONE',  ( -97.69448315145120887, 134.5322016254652056, 15.49925189408050841 ) ) ;
#20328 = ORIENTED_EDGE ( 'NONE', *, *, #2266, .F. ) ;
#20329 = LINE ( 'NONE', #9128, #10359 ) ;
#20330 = VERTEX_POINT ( 'NONE', #6250 ) ;
#20331 = VECTOR ( 'NONE', #28193, 1000.000000000000000 ) ;
#20332 = ORIENTED_EDGE ( 'NONE', *, *, #9061, .T. ) ;
#20333 = CARTESIAN_POINT ( 'NONE',  ( 134.9999999999998579, 220.0000000000000284, 90.00000000000002842 ) ) ;
#20334 = VERTEX_POINT ( 'NONE', #12875 ) ;
#20335 = CIRCLE ( 'NONE', #5647, 6.025000000000002132 ) ;
#20336 = ORIENTED_EDGE ( 'NONE', *, *, #3021, .F. ) ;
#20337 = VERTEX_POINT ( 'NONE', #12737 ) ;
#20338 = VECTOR ( 'NONE', #18898, 1000.000000000000000 ) ;
#20339 = CARTESIAN_POINT ( 'NONE',  ( 99.67744569820828815, 242.4823527582436498, 13.37113024292247054 ) ) ;
#20340 = DIRECTION ( 'NONE',  ( -1.000000000000000000, -8.673617379884036705E-17, 0.000000000000000000 ) ) ;
#20341 = CARTESIAN_POINT ( 'NONE',  ( 157.4999999999996874, 266.3956876388795649, -45.00000000000000000 ) ) ;
#20342 = B_SPLINE_CURVE_WITH_KNOTS ( 'NONE', 3,
 ( #23671, #25256, #7873, #10176, #16643, #8155, #18790, #10314, #6143, #12627, #20945, #27535, #21083, #12763, #27678, #23382, #21366, #16918, #8015, #16782, #12484, #27817, #21225, #23526, #3976, #19353, #5853, #14629, #1549, #27956 ),
 .UNSPECIFIED., .F., .F.,
 ( 4, 2, 2, 2, 2, 2, 2, 2, 2, 2, 2, 2, 2, 2, 4 ),
 ( 0.000000000000000000, 0.002307319121158361939, 0.004614638242316723878, 0.006921957363475085383, 0.009229276484633447755, 0.01384391472695016383, 0.01615123384810852533, 0.01845855296926688857, 0.02307319121158360464, 0.02538051033274192972, 0.02768782945390025133, 0.02999514857505857987, 0.03114880813563770945, 0.03230246769621684250, 0.03691710593853337469 ),
 .UNSPECIFIED. ) ;
#20343 = CARTESIAN_POINT ( 'NONE',  ( 98.15430812615089451, 116.0637945823775112, -78.75000000033432457 ) ) ;
#20344 = EDGE_CURVE ( 'NONE', #16524, #4562, #27402, .T. ) ;
#20345 = DIRECTION ( 'NONE',  ( 1.000000000000000000, -0.000000000000000000, -0.000000000000000000 ) ) ;
#20346 = CARTESIAN_POINT ( 'NONE',  ( 79.99999999999994316, -100.0000000000000284, 70.00000000000001421 ) ) ;
#20347 = DIRECTION ( 'NONE',  ( 0.2588190451025252359, 0.9659258262890672020, -0.000000000000000000 ) ) ;
#20348 = DIRECTION ( 'NONE',  ( 0.000000000000000000, 0.000000000000000000, 1.000000000000000000 ) ) ;
#20349 = CARTESIAN_POINT ( 'NONE',  ( -276.2395898676904835, -169.9272804698039749, 107.3924858170726964 ) ) ;
#20350 = CARTESIAN_POINT ( 'NONE',  ( -24.33210486176665910, 0.000000000000000000, 99.00000000000000000 ) ) ;
#20351 = LINE ( 'NONE', #19921, #8876 ) ;
#20352 = ORIENTED_EDGE ( 'NONE', *, *, #16744, .T. ) ;
#20353 = VECTOR ( 'NONE', #23698, 1000.000000000000227 ) ;
#20354 = PLANE ( 'NONE',  #12890 ) ;
#20355 = EDGE_CURVE ( 'NONE', #14898, #14664, #10568, .T. ) ;
#20356 = AXIS2_PLACEMENT_3D ( 'NONE', #15851, #4194, #12985 ) ;
#20357 = EDGE_CURVE ( 'NONE', #21673, #10576, #10854, .T. ) ;
#20358 = DIRECTION ( 'NONE',  ( -0.5241030343220994814, -0.8516548651973804285, -0.000000000000000000 ) ) ;
#20359 = FACE_OUTER_BOUND ( 'NONE', #22940, .T. ) ;
#20360 = CARTESIAN_POINT ( 'NONE',  ( -210.0000000000000568, -160.0000000000002558, -110.0000000000000284 ) ) ;
#20361 = CIRCLE ( 'NONE', #24956, 10.53396790234564406 ) ;
#20362 = ORIENTED_EDGE ( 'NONE', *, *, #19597, .T. ) ;
#20363 = PRODUCT_DEFINITION ( 'UNKNOWN', '', #12944, #23839 ) ;
#20364 = CARTESIAN_POINT ( 'NONE',  ( 109.9999999999998863, 260.0000000000000000, -45.00000000000000000 ) ) ;
#20365 = ORIENTED_EDGE ( 'NONE', *, *, #26185, .T. ) ;
#20366 = ORIENTED_EDGE ( 'NONE', *, *, #5684, .F. ) ;
#20367 = ORIENTED_EDGE ( 'NONE', *, *, #735, .T. ) ;
#20368 = EDGE_LOOP ( 'NONE', ( #13369, #21637, #21050, #646 ) ) ;
#20369 = ORIENTED_EDGE ( 'NONE', *, *, #25821, .T. ) ;
#20370 = DIRECTION ( 'NONE',  ( -0.000000000000000000, 1.000000000000000000, -1.387778780781445429E-16 ) ) ;
#20371 = CONICAL_SURFACE ( 'NONE', #24043, 30.00000000000001421, 0.7853981633974500554 ) ;
#20372 = CARTESIAN_POINT ( 'NONE',  ( 157.4999999999998579, 196.1751874286831026, 45.00000000000000000 ) ) ;
#20373 = CARTESIAN_POINT ( 'NONE',  ( 91.50131282131302157, 230.4711573898007373, 17.28742291603535364 ) ) ;
#20374 = CARTESIAN_POINT ( 'NONE',  ( -67.45409458357327992, 135.5144413978513001, -13.65941681365853277 ) ) ;
#20375 = EDGE_CURVE ( 'NONE', #21445, #25157, #7745, .T. ) ;
#20376 = CARTESIAN_POINT ( 'NONE',  ( 157.4999999999998010, 233.7933125412885147, 45.00000000000000000 ) ) ;
#20377 = CARTESIAN_POINT ( 'NONE',  ( -208.5235512171359176, 74.87362916051154116, 38.25286048366049840 ) ) ;
#20378 = DIRECTION ( 'NONE',  ( 0.8916010070293484135, -0.4528218681382910060, 0.000000000000000000 ) ) ;
#20379 = EDGE_CURVE ( 'NONE', #11335, #15093, #18019, .T. ) ;
#20380 = CARTESIAN_POINT ( 'NONE',  ( 12.13064872364015123, -50.00000000000007105, 98.28427124746193044 ) ) ;
#20381 = CARTESIAN_POINT ( 'NONE',  ( 217.4999999999996305, 83.06687458711267880, -36.86484227207694175 ) ) ;
#20382 = DIRECTION ( 'NONE',  ( -1.000000000000000000, 0.000000000000000000, 0.000000000000000000 ) ) ;
#20383 = LINE ( 'NONE', #17406, #17006 ) ;
#20384 = LINE ( 'NONE', #9334, #14604 ) ;
#20385 = CARTESIAN_POINT ( 'NONE',  ( -210.0000000000000284, -40.00000000000005684, 70.00000000000001421 ) ) ;
#20386 = CARTESIAN_POINT ( 'NONE',  ( -20.22836655706693776, 129.6440146278404768, 16.81209664567878548 ) ) ;
#20387 = EDGE_CURVE ( 'NONE', #4329, #1247, #16513, .T. ) ;
#20388 = DIRECTION ( 'NONE',  ( -0.05364526231778204285, 0.9985600561963493549, 0.000000000000000000 ) ) ;
#20389 = CARTESIAN_POINT ( 'NONE',  ( 109.9999999999999574, -120.0000000000000711, -70.00000000000001421 ) ) ;
#20390 = DIRECTION ( 'NONE',  ( -0.000000000000000000, -0.000000000000000000, -1.000000000000000000 ) ) ;
#20392 = ORIENTED_EDGE ( 'NONE', *, *, #16147, .T. ) ;
#20391 = VERTEX_POINT ( 'NONE', #8415 ) ;
#20393 = AXIS2_PLACEMENT_3D ( 'NONE', #10661, #17122, #28165 ) ;
#20394 = CARTESIAN_POINT ( 'NONE',  ( -220.0118810049154661, 86.25235459150694339, -18.72563439332759216 ) ) ;
#20395 = ADVANCED_FACE ( 'NONE', ( #3949 ), #25264, .F. ) ;
#20396 = DIRECTION ( 'NONE',  ( -0.000000000000000000, -0.000000000000000000, -1.000000000000000000 ) ) ;
#20397 = VERTEX_POINT ( 'NONE', #20953 ) ;
#20398 = ORIENTED_EDGE ( 'NONE', *, *, #14170, .F. ) ;
#20399 = CARTESIAN_POINT ( 'NONE',  ( 158.0000000000009379, 116.1771246922112653, 45.00000000000000000 ) ) ;
#20400 = CARTESIAN_POINT ( 'NONE',  ( -138.7249983104375133, 128.6417097633065225, 17.20246859800720429 ) ) ;
#20401 = VERTEX_POINT ( 'NONE', #10428 ) ;
#20402 = ORIENTED_EDGE ( 'NONE', *, *, #1365, .T. ) ;
#20403 = PLANE ( 'NONE',  #23436 ) ;
#20404 = EDGE_CURVE ( 'NONE', #1347, #26566, #12069, .T. ) ;
#20405 = DIRECTION ( 'NONE',  ( 1.000000000000000000, 0.000000000000000000, -0.000000000000000000 ) ) ;
#20406 = LINE ( 'NONE', #736, #15123 ) ;
#20407 = CARTESIAN_POINT ( 'NONE',  ( -68.57415822541635464, -23.01420295945612082, 80.00000000000001421 ) ) ;
#20408 = VECTOR ( 'NONE', #7350, 1000.000000000000000 ) ;
#20409 = LINE ( 'NONE', #5182, #14867 ) ;
#20410 = EDGE_CURVE ( 'NONE', #1799, #21665, #27928, .T. ) ;
#20411 = CARTESIAN_POINT ( 'NONE',  ( 134.9999999999998579, 220.0000000000000284, -122.9999999999999574 ) ) ;
#20412 = AXIS2_PLACEMENT_3D ( 'NONE', #28179, #14995, #8524 ) ;
#20413 = DIRECTION ( 'NONE',  ( 1.530283246943720875E-16, -1.000000000000000000, 0.000000000000000000 ) ) ;
#20414 = CARTESIAN_POINT ( 'NONE',  ( -216.1549772618016334, 59.20708407665082262, -28.62293862808999734 ) ) ;
#20415 = LINE ( 'NONE', #13976, #24728 ) ;
#20416 = DIRECTION ( 'NONE',  ( -0.000000000000000000, -0.000000000000000000, -1.000000000000000000 ) ) ;
#20417 = PLANE ( 'NONE',  #17996 ) ;
#20418 = CARTESIAN_POINT ( 'NONE',  ( -274.7557459110829541, -165.0000000000001137, -86.12025961983451339 ) ) ;
#20419 = ORIENTED_EDGE ( 'NONE', *, *, #12791, .F. ) ;
#20420 = FACE_OUTER_BOUND ( 'NONE', #24391, .T. ) ;
#20421 = ADVANCED_FACE ( 'NONE', ( #16377 ), #17307, .F. ) ;
#20422 = EDGE_CURVE ( 'NONE', #14865, #7880, #17027, .T. ) ;
#20423 = CARTESIAN_POINT ( 'NONE',  ( 65.00000000000000000, -120.0000000000000995, -64.00000000000000000 ) ) ;
#20424 = CARTESIAN_POINT ( 'NONE',  ( 115.5814157129579058, 207.6339745962153245, 45.00000000000000000 ) ) ;
#20425 = ORIENTED_EDGE ( 'NONE', *, *, #13350, .T. ) ;
#20426 =( NAMED_UNIT ( * ) SI_UNIT ( $, .STERADIAN. ) SOLID_ANGLE_UNIT ( ) );
#20427 = AXIS2_PLACEMENT_3D ( 'NONE', #11601, #808, #20340 ) ;
#20428 = EDGE_LOOP ( 'NONE', ( #7340, #11143, #20116, #3417 ) ) ;
#20429 = CIRCLE ( 'NONE', #11252, 80.00000000000000000 ) ;
#20430 = VECTOR ( 'NONE', #25960, 1000.000000000000114 ) ;
#20431 = CARTESIAN_POINT ( 'NONE',  ( 158.0000000000017053, 43.44874947450702507, -45.00000000000000000 ) ) ;
#20432 = DIRECTION ( 'NONE',  ( -1.000000000000000000, 0.000000000000000000, -0.000000000000000000 ) ) ;
#20433 = ORIENTED_EDGE ( 'NONE', *, *, #18284, .T. ) ;
#20434 = AXIS2_PLACEMENT_3D ( 'NONE', #23999, #19966, #26564 ) ;
#20436 = EDGE_CURVE ( 'NONE', #20107, #20401, #18938, .T. ) ;
#20435 = ORIENTED_EDGE ( 'NONE', *, *, #21293, .T. ) ;
#20437 = LINE ( 'NONE', #26760, #9051 ) ;
#20438 = LINE ( 'NONE', #16140, #13029 ) ;
#20439 = CARTESIAN_POINT ( 'NONE',  ( -210.0000000000000568, -216.9546086794800317, -90.40281535134946012 ) ) ;
#20440 = ORIENTED_EDGE ( 'NONE', *, *, #20956, .T. ) ;
#20441 = DIRECTION ( 'NONE',  ( -1.000000000000000000, 0.000000000000000000, -0.000000000000000000 ) ) ;
#20442 = ORIENTED_EDGE ( 'NONE', *, *, #12133, .T. ) ;
#20443 = DIRECTION ( 'NONE',  ( 1.000000000000000000, 0.000000000000000000, -0.000000000000000000 ) ) ;
#20444 = EDGE_CURVE ( 'NONE', #12189, #17779, #28085, .T. ) ;
#20445 = CARTESIAN_POINT ( 'NONE',  ( 158.0000000000005116, 158.8109998198309825, -45.00000000000000000 ) ) ;
#20446 = CIRCLE ( 'NONE', #13567, 22.49999999999997868 ) ;
#20447 = EDGE_CURVE ( 'NONE', #15242, #20027, #17879, .T. ) ;
#20448 = CARTESIAN_POINT ( 'NONE',  ( -160.0000000000000284, 221.6666220619077876, -15.00000000000000000 ) ) ;
#20449 = CARTESIAN_POINT ( 'NONE',  ( -1.286094456368339189, 135.5506476309248569, -13.59701399039920844 ) ) ;
#20450 = AXIS2_PLACEMENT_3D ( 'NONE', #24803, #15912, #5257 ) ;
#20451 = PLANE ( 'NONE',  #20584 ) ;
#20452 = AXIS2_PLACEMENT_3D ( 'NONE', #6928, #22596, #476 ) ;
#20453 = CARTESIAN_POINT ( 'NONE',  ( 158.0000000000007390, 135.7322497447605656, 45.00000000000000000 ) ) ;
#20454 = LINE ( 'NONE', #18017, #26757 ) ;
#20455 = ORIENTED_EDGE ( 'NONE', *, *, #7697, .T. ) ;
#20456 = FACE_OUTER_BOUND ( 'NONE', #3108, .T. ) ;
#20457 = VECTOR ( 'NONE', #25590, 1000.000000000000000 ) ;
#20458 = CARTESIAN_POINT ( 'NONE',  ( -58.76345596729049703, 58.76345596729049703, 45.00000000000000000 ) ) ;
#20459 = DIRECTION ( 'NONE',  ( 1.000000000000000000, 0.000000000000000000, -0.000000000000000000 ) ) ;
#20460 = CARTESIAN_POINT ( 'NONE',  ( 157.4999999999998579, 65.76568703831686946, -45.00000000000000000 ) ) ;
#20461 = ORIENTED_EDGE ( 'NONE', *, *, #16804, .T. ) ;
#20462 = CARTESIAN_POINT ( 'NONE',  ( 282.4999999999996589, 19.41075299063184900, 80.49671038392669686 ) ) ;
#20463 = ORIENTED_EDGE ( 'NONE', *, *, #25620, .F. ) ;
#20464 = CARTESIAN_POINT ( 'NONE',  ( 134.9999999999998579, 220.0000000000000284, -90.00000000000002842 ) ) ;
#20465 = CARTESIAN_POINT ( 'NONE',  ( 157.4999999999998579, 130.9704372334999789, 45.00000000000000000 ) ) ;
#20466 = FACE_OUTER_BOUND ( 'NONE', #4846, .T. ) ;
#20467 = ORIENTED_EDGE ( 'NONE', *, *, #19163, .F. ) ;
#20468 = CARTESIAN_POINT ( 'NONE',  ( 232.4999999999996305, 133.0668745871126930, -30.86484227207697018 ) ) ;
#20469 = PLANE ( 'NONE',  #26234 ) ;
#20470 = ORIENTED_EDGE ( 'NONE', *, *, #16393, .T. ) ;
#20471 = DIRECTION ( 'NONE',  ( 1.000000000000000000, 0.000000000000000000, 0.000000000000000000 ) ) ;
#20472 = DIRECTION ( 'NONE',  ( 0.4528218681382463751, 0.8916010070293711731, -0.000000000000000000 ) ) ;
#20473 = ORIENTED_EDGE ( 'NONE', *, *, #27717, .F. ) ;
#20474 = VECTOR ( 'NONE', #12531, 1000.000000000000000 ) ;
#20475 = VERTEX_POINT ( 'NONE', #8977 ) ;
#20476 = CARTESIAN_POINT ( 'NONE',  ( -17.24491960465745777, -18.01420295945611727, 100.0000000000000000 ) ) ;
#20477 = ORIENTED_EDGE ( 'NONE', *, *, #28050, .F. ) ;
#20478 = ORIENTED_EDGE ( 'NONE', *, *, #8847, .T. ) ;
#20479 = VECTOR ( 'NONE', #19036, 1000.000000000000000 ) ;
#20480 = ORIENTED_EDGE ( 'NONE', *, *, #20675, .F. ) ;
#20481 = ADVANCED_FACE ( 'NONE', ( #13437 ), #4798, .F. ) ;
#20482 = CARTESIAN_POINT ( 'NONE',  ( 109.8651760759796332, 256.6126121035342749, 42.06544492438914773 ) ) ;
#20483 = ADVANCED_FACE ( 'NONE', ( #24204 ), #13299, .F. ) ;
#20484 = CARTESIAN_POINT ( 'NONE',  ( 157.9999999999997158, 258.6181251126050711, -45.00000000000000000 ) ) ;
#20485 = CARTESIAN_POINT ( 'NONE',  ( -228.3260857049913284, 133.0445111367241680, -15.00000000000000355 ) ) ;
#20486 = CARTESIAN_POINT ( 'NONE',  ( 157.9999999999997726, 246.0787500750700474, 45.00000000000000000 ) ) ;
#20487 = DIRECTION ( 'NONE',  ( -0.000000000000000000, -0.000000000000000000, -1.000000000000000000 ) ) ;
#20488 = DIRECTION ( 'NONE',  ( -0.8314772792026874360, 0.5555587585212711232, 0.000000000000000000 ) ) ;
#20489 = LINE ( 'NONE', #814, #25983 ) ;
#20490 = PLANE ( 'NONE',  #26385 ) ;
#20491 = CARTESIAN_POINT ( 'NONE',  ( 113.4999999999998863, 220.0000000000000284, 99.00000000000001421 ) ) ;
#20492 = CARTESIAN_POINT ( 'NONE',  ( 157.4999999999995168, 208.7145624662163925, 45.00000000000000000 ) ) ;
#20493 = DIRECTION ( 'NONE',  ( 0.000000000000000000, 0.000000000000000000, -1.000000000000000000 ) ) ;
#20494 = VECTOR ( 'NONE', #22165, 1000.000000000000114 ) ;
#20495 = ORIENTED_EDGE ( 'NONE', *, *, #5523, .T. ) ;
#20496 = EDGE_CURVE ( 'NONE', #23733, #24388, #15455, .T. ) ;
#20497 = CARTESIAN_POINT ( 'NONE',  ( 1.250275373174976279, -1.250000000000000444, 7.480737022738205511 ) ) ;
#20498 = DIRECTION ( 'NONE',  ( 0.7440215159218921404, -0.6681556583950251094, 0.000000000000000000 ) ) ;
#20499 = LINE ( 'NONE', #18355, #19346 ) ;
#20500 = ORIENTED_EDGE ( 'NONE', *, *, #7862, .F. ) ;
#20501 = DIRECTION ( 'NONE',  ( -0.000000000000000000, -0.000000000000000000, 1.000000000000000000 ) ) ;
#20502 = ORIENTED_EDGE ( 'NONE', *, *, #20404, .T. ) ;
#20503 = EDGE_CURVE ( 'NONE', #9458, #11526, #26786, .T. ) ;
#20504 = CARTESIAN_POINT ( 'NONE',  ( 157.4999999999998295, 40.68693696324645970, 45.00000000000000000 ) ) ;
#20505 = VERTEX_POINT ( 'NONE', #17448 ) ;
#20506 = VERTEX_POINT ( 'NONE', #24339 ) ;
#20507 = VERTEX_POINT ( 'NONE', #4509 ) ;
#20508 = EDGE_CURVE ( 'NONE', #15103, #8705, #8695, .T. ) ;
#20509 = ORIENTED_EDGE ( 'NONE', *, *, #25785, .F. ) ;
#20510 = DIRECTION ( 'NONE',  ( 0.8916010070297439860, -0.4528218681375119070, 0.000000000000000000 ) ) ;
#20511 = AXIS2_PLACEMENT_3D ( 'NONE', #23128, #1283, #14236 ) ;
#20512 = CARTESIAN_POINT ( 'NONE',  ( 187.4999999999996305, 258.6181251126050711, -5.999999999999991118 ) ) ;
#20513 = CARTESIAN_POINT ( 'NONE',  ( 157.4999999999998579, 181.1279373836408411, 45.00000000000000000 ) ) ;
#20514 = ADVANCED_FACE ( 'NONE', ( #15742 ), #2352, .F. ) ;
#20515 = AXIS2_PLACEMENT_3D ( 'NONE', #3399, #14480, #16773 ) ;
#20516 = EDGE_CURVE ( 'NONE', #19223, #3225, #9329, .T. ) ;
#20517 = CARTESIAN_POINT ( 'NONE',  ( -77.62792406888256380, 134.6615905559135058, -15.47644436303202653 ) ) ;
#20518 = CARTESIAN_POINT ( 'NONE',  ( -38.15943738855941803, 129.9964879898109587, 15.32333988264501556 ) ) ;
#20519 = CARTESIAN_POINT ( 'NONE',  ( -207.4994891700685002, 75.60264349980251097, 44.78213549412046746 ) ) ;
#20520 = CARTESIAN_POINT ( 'NONE',  ( -210.0000000000000568, -220.0000000000000853, 90.87829376371914236 ) ) ;
#20521 = CARTESIAN_POINT ( 'NONE',  ( -108.0012317229447376, 135.2240360019066259, -13.71905899893544145 ) ) ;
#20522 = CARTESIAN_POINT ( 'NONE',  ( -12.24491960465745599, -23.01420295945612082, 100.0000000000000000 ) ) ;
#20523 = CARTESIAN_POINT ( 'NONE',  ( 121.6232796275294277, 239.4748271322486630, 45.00000000000000000 ) ) ;
#20524 = DIRECTION ( 'NONE',  ( 0.8916010070299672519, -0.4528218681370723142, 0.000000000000000000 ) ) ;
#20525 = FACE_OUTER_BOUND ( 'NONE', #23198, .T. ) ;
#20526 = CARTESIAN_POINT ( 'NONE',  ( 90.92319367352486381, 112.0484670279021771, 72.65625000014701129 ) ) ;
#20527 = DIRECTION ( 'NONE',  ( -0.000000000000000000, -1.000000000000000000, -0.000000000000000000 ) ) ;
#20528 = CARTESIAN_POINT ( 'NONE',  ( 82.91040908012101340, 80.00000000661717081, -100.0000000000000142 ) ) ;
#20529 = DIRECTION ( 'NONE',  ( 0.000000000000000000, 0.000000000000000000, 1.000000000000000000 ) ) ;
#20531 = ORIENTED_EDGE ( 'NONE', *, *, #15962, .F. ) ;
#20530 = ORIENTED_EDGE ( 'NONE', *, *, #14545, .F. ) ;
#20532 = VECTOR ( 'NONE', #4990, 1000.000000000000000 ) ;
#20533 = CARTESIAN_POINT ( 'NONE',  ( -209.3667759261723234, 88.45076432448455250, -25.75869258754447699 ) ) ;
#20534 = DIRECTION ( 'NONE',  ( 0.000000000000000000, -1.000000000000000000, 0.000000000000000000 ) ) ;
#20535 = ORIENTED_EDGE ( 'NONE', *, *, #831, .T. ) ;
#20536 = EDGE_LOOP ( 'NONE', ( #20442, #536, #14921, #27432 ) ) ;
#20537 = EDGE_CURVE ( 'NONE', #23894, #26741, #13585, .T. ) ;
#20538 = EDGE_CURVE ( 'NONE', #7480, #19401, #20335, .T. ) ;
#20539 = DIRECTION ( 'NONE',  ( -0.000000000000000000, 0.000000000000000000, -1.000000000000000000 ) ) ;
#20540 = CARTESIAN_POINT ( 'NONE',  ( -62.71494712997262155, 133.3675451889207864, 15.73174655005644595 ) ) ;
#20541 = ORIENTED_EDGE ( 'NONE', *, *, #14015, .F. ) ;
#20542 = EDGE_LOOP ( 'NONE', ( #4240, #1768, #15330, #8372, #10664 ) ) ;
#20543 = CARTESIAN_POINT ( 'NONE',  ( -163.8236447719811224, 118.1194741415192482, -24.35161506463292724 ) ) ;
#20544 = DIRECTION ( 'NONE',  ( 0.8916010070293383105, -0.4528218681383106015, 0.000000000000000000 ) ) ;
#20545 = AXIS2_PLACEMENT_3D ( 'NONE', #19386, #15518, #15379 ) ;
#20546 = EDGE_CURVE ( 'NONE', #19128, #12951, #15889, .T. ) ;
#20547 = DIRECTION ( 'NONE',  ( 0.4528218681370723142, 0.8916010070299673629, -0.000000000000000000 ) ) ;
#20548 = DIRECTION ( 'NONE',  ( 0.000000000000000000, 0.000000000000000000, 1.000000000000000000 ) ) ;
#20549 = PRODUCT_RELATED_PRODUCT_CATEGORY ( 'part', '', ( #18972 ) ) ;
#20550 = CARTESIAN_POINT ( 'NONE',  ( 20.92655468430566756, 155.3461090732848220, -13.00000000000000000 ) ) ;
#20551 = DIRECTION ( 'NONE',  ( 1.000000000000000000, 2.602085213965211135E-16, -0.000000000000000000 ) ) ;
#20552 = CARTESIAN_POINT ( 'NONE',  ( -208.5306448315634213, 60.03373823553869926, -18.45924612779791474 ) ) ;
#20554 = CARTESIAN_POINT ( 'NONE',  ( 112.4999999999998863, 220.0000000000000284, -84.99999999999997158 ) ) ;
#20553 = CIRCLE ( 'NONE', #5422, 5.000000000000004441 ) ;
#20555 = LINE ( 'NONE', #27711, #20700 ) ;
#20556 = CARTESIAN_POINT ( 'NONE',  ( -305.0000000000001137, -157.0000000000000284, -59.99999999999987210 ) ) ;
#20557 = DIRECTION ( 'NONE',  ( -0.000000000000000000, 0.000000000000000000, -1.000000000000000000 ) ) ;
#20558 = ORIENTED_EDGE ( 'NONE', *, *, #24799, .F. ) ;
#20559 = DIRECTION ( 'NONE',  ( -0.8916010070297749612, -0.4528218681374510668, 0.000000000000000000 ) ) ;
#20560 = VECTOR ( 'NONE', #11611, 1000.000000000000114 ) ;
#20561 = CARTESIAN_POINT ( 'NONE',  ( -235.8599852676175601, 67.86969485656919687, 15.13802962878585490 ) ) ;
#20562 = AXIS2_PLACEMENT_3D ( 'NONE', #5785, #25596, #27884 ) ;
#20563 = LINE ( 'NONE', #1025, #13577 ) ;
#20564 = ORIENTED_EDGE ( 'NONE', *, *, #8251, .T. ) ;
#20565 = APPLICATION_PROTOCOL_DEFINITION ( 'draft international standard', 'automotive_design', 1998, #21209 ) ;
#20566 = ORIENTED_EDGE ( 'NONE', *, *, #28115, .T. ) ;
#20567 = EDGE_CURVE ( 'NONE', #15393, #12113, #360, .T. ) ;
#20568 = EDGE_CURVE ( 'NONE', #26119, #24246, #9118, .T. ) ;
#20569 = CARTESIAN_POINT ( 'NONE',  ( 109.9999999999999289, 140.0000000000000000, 100.0000000000000142 ) ) ;
#20570 = DIRECTION ( 'NONE',  ( 1.000000000000000000, 0.000000000000000000, 0.000000000000000000 ) ) ;
#20571 = VERTEX_POINT ( 'NONE', #9266 ) ;
#20572 = VERTEX_POINT ( 'NONE', #11577 ) ;
#20573 = CARTESIAN_POINT ( 'NONE',  ( 157.4999999999998579, 103.3838121509225090, 45.00000000000000000 ) ) ;
#20574 = CARTESIAN_POINT ( 'NONE',  ( 135.1062353973271968, 7.258260926501912458, -45.00000000000000000 ) ) ;
#20575 = VECTOR ( 'NONE', #21689, 1000.000000000000000 ) ;
#20576 = CARTESIAN_POINT ( 'NONE',  ( 157.4999999999998579, 135.9861872485140850, 45.00000000000000000 ) ) ;
#20577 = VERTEX_POINT ( 'NONE', #6535 ) ;
#20578 = CARTESIAN_POINT ( 'NONE',  ( 109.9999999999999432, 2.035408878479452500E-14, -90.00000000000004263 ) ) ;
#20579 = ORIENTED_EDGE ( 'NONE', *, *, #3155, .F. ) ;
#20580 = CARTESIAN_POINT ( 'NONE',  ( -59.48697296830715686, 2.336311854928212824E-15, 99.00000000000000000 ) ) ;
#20581 = CIRCLE ( 'NONE', #26537, 17.93072811908088937 ) ;
#20582 = EDGE_CURVE ( 'NONE', #10648, #27544, #24634, .T. ) ;
#20583 = EDGE_CURVE ( 'NONE', #15830, #26119, #7022, .T. ) ;
#20584 = AXIS2_PLACEMENT_3D ( 'NONE', #24905, #5219, #9541 ) ;
#20585 = DIRECTION ( 'NONE',  ( 0.8916010070293584056, -0.4528218681382712996, 0.000000000000000000 ) ) ;
#20586 = DIRECTION ( 'NONE',  ( -0.000000000000000000, -0.000000000000000000, -1.000000000000000000 ) ) ;
#20587 = CARTESIAN_POINT ( 'NONE',  ( -33.95367337125702534, 128.1958190094148620, -17.41813228564776139 ) ) ;
#20588 = DIRECTION ( 'NONE',  ( 0.000000000000000000, -1.000000000000000000, 0.000000000000000000 ) ) ;
#20589 = VECTOR ( 'NONE', #19696, 1000.000000000000000 ) ;
#20590 = CARTESIAN_POINT ( 'NONE',  ( -265.0574300291106056, -165.8879864452689219, -89.57768297750722297 ) ) ;
#20591 = CARTESIAN_POINT ( 'NONE',  ( 161.1767780239350145, 205.3395095159081336, -138.9999999999999432 ) ) ;
#20592 = ORIENTED_EDGE ( 'NONE', *, *, #1320, .T. ) ;
#20593 = CARTESIAN_POINT ( 'NONE',  ( 156.9574749595459195, 226.9187638636467739, 45.00000000000000000 ) ) ;
#20594 = FACE_OUTER_BOUND ( 'NONE', #21616, .T. ) ;
#20595 = CARTESIAN_POINT ( 'NONE',  ( 158.0000000000012506, 86.08262460212675649, -45.00000000000000000 ) ) ;
#20596 = EDGE_LOOP ( 'NONE', ( #26785, #27278, #19445, #25100 ) ) ;
#20597 = EDGE_CURVE ( 'NONE', #27997, #17680, #10996, .T. ) ;
#20598 = DIRECTION ( 'NONE',  ( 0.000000000000000000, 0.000000000000000000, -1.000000000000000000 ) ) ;
#20599 = ORIENTED_EDGE ( 'NONE', *, *, #16628, .F. ) ;
#20600 = EDGE_CURVE ( 'NONE', #17312, #9431, #9797, .T. ) ;
#20601 = VECTOR ( 'NONE', #23319, 1000.000000000000000 ) ;
#20602 = CARTESIAN_POINT ( 'NONE',  ( 157.9999999999996589, 279.1890001801680796, -45.00000000000000000 ) ) ;
#20603 = DIRECTION ( 'NONE',  ( 1.000000000000000000, 0.000000000000000000, 0.000000000000000000 ) ) ;
#20604 = CARTESIAN_POINT ( 'NONE',  ( 177.1897033089359184, 197.3087408678716770, -45.00000000000000000 ) ) ;
#20605 = ORIENTED_EDGE ( 'NONE', *, *, #24879, .T. ) ;
#20606 = CARTESIAN_POINT ( 'NONE',  ( 167.4999999999996589, 526.4263741777961059, 74.99999999999995737 ) ) ;
#20607 = LINE ( 'NONE', #9836, #11588 ) ;
#20608 = ORIENTED_EDGE ( 'NONE', *, *, #26745, .T. ) ;
#20609 = CIRCLE ( 'NONE', #26115, 44.99999999999999289 ) ;
#20610 = CARTESIAN_POINT ( 'NONE',  ( 134.9999999999998579, 171.5103103742661688, 84.99999999999995737 ) ) ;
#20611 = DIRECTION ( 'NONE',  ( 0.000000000000000000, -1.000000000000000000, 0.000000000000000000 ) ) ;
#20612 = VERTEX_POINT ( 'NONE', #27336 ) ;
#20613 = EDGE_LOOP ( 'NONE', ( #4806, #8317, #409, #14610 ) ) ;
#20614 = AXIS2_PLACEMENT_3D ( 'NONE', #19945, #6447, #4565 ) ;
#20615 = CARTESIAN_POINT ( 'NONE',  ( 157.4999999999998579, 166.0806873385985796, 45.00000000000000000 ) ) ;
#20616 = ORIENTED_EDGE ( 'NONE', *, *, #10956, .T. ) ;
#20617 = ORIENTED_EDGE ( 'NONE', *, *, #21127, .F. ) ;
#20618 = ORIENTED_EDGE ( 'NONE', *, *, #13101, .F. ) ;
#20619 = DIRECTION ( 'NONE',  ( -0.000000000000000000, -0.000000000000000000, -1.000000000000000000 ) ) ;
#20620 = EDGE_CURVE ( 'NONE', #19969, #860, #11721, .T. ) ;
#20621 = VECTOR ( 'NONE', #10495, 1000.000000000000000 ) ;
#20622 = DIRECTION ( 'NONE',  ( 0.000000000000000000, -1.000000000000000000, 0.000000000000000000 ) ) ;
#20623 = B_SPLINE_CURVE_WITH_KNOTS ( 'NONE', 3,
 ( #1181, #27181, #23159, #20439, #9947, #18704 ),
 .UNSPECIFIED., .F., .F.,
 ( 4, 2, 4 ),
 ( 0.000000000000000000, 0.004615224477119856880, 0.009230448954239713760 ),
 .UNSPECIFIED. ) ;
#20624 = AXIS2_PLACEMENT_3D ( 'NONE', #9811, #18571, #27316 ) ;
#20625 = CARTESIAN_POINT ( 'NONE',  ( -175.0000000000000000, -120.0250000000001762, 64.00000000000001421 ) ) ;
#20626 = DIRECTION ( 'NONE',  ( -0.8916010070293409751, -0.4528218681383056610, 0.000000000000000000 ) ) ;
#20627 = VECTOR ( 'NONE', #5828, 1000.000000000000000 ) ;
#20628 = DIRECTION ( 'NONE',  ( -0.000000000000000000, -0.000000000000000000, -1.000000000000000000 ) ) ;
#20629 = CARTESIAN_POINT ( 'NONE',  ( 158.0000000000004832, 163.3188748273380213, -45.00000000000000000 ) ) ;
#20630 = DIRECTION ( 'NONE',  ( -0.05364526231779676024, -0.9985600561963485777, 0.000000000000000000 ) ) ;
#20631 = CARTESIAN_POINT ( 'NONE',  ( 157.9999999999996589, 274.1732501651540588, 45.00000000000000000 ) ) ;
#20632 = CARTESIAN_POINT ( 'NONE',  ( -41.04971513216914047, 194.3765543069588659, 45.00000000000000000 ) ) ;
#20633 = DIRECTION ( 'NONE',  ( 0.000000000000000000, -1.000000000000000000, 0.000000000000000000 ) ) ;
#20634 = DIRECTION ( 'NONE',  ( 0.000000000000000000, 0.000000000000000000, -1.000000000000000000 ) ) ;
#20635 = ORIENTED_EDGE ( 'NONE', *, *, #25702, .F. ) ;
#20636 = VECTOR ( 'NONE', #5567, 1000.000000000000000 ) ;
#20637 = DIRECTION ( 'NONE',  ( 0.000000000000000000, -1.000000000000000000, -1.214306433183764966E-16 ) ) ;
#20638 = CARTESIAN_POINT ( 'NONE',  ( 9.999999999999749534, 90.00000000000001421, 98.28427124746191623 ) ) ;
#20639 = DIRECTION ( 'NONE',  ( 0.4528218681380302146, -0.8916010070294808632, 0.000000000000000000 ) ) ;
#20640 = ORIENTED_EDGE ( 'NONE', *, *, #25752, .T. ) ;
#20641 = EDGE_CURVE ( 'NONE', #583, #20671, #5657, .T. ) ;
#20642 = ADVANCED_FACE ( 'NONE', ( #9414 ), #24472, .T. ) ;
#20643 = TOROIDAL_SURFACE ( 'NONE', #4125, 79.71075545852265520, 9.999999999999996447 ) ;
#20644 = DIRECTION ( 'NONE',  ( -1.000000000000000000, 0.000000000000000000, 0.000000000000000000 ) ) ;
#20645 = ORIENTED_EDGE ( 'NONE', *, *, #22190, .T. ) ;
#20646 = DIRECTION ( 'NONE',  ( -1.000000000000000000, -1.321694076934710155E-16, 0.000000000000000000 ) ) ;
#20647 = EDGE_CURVE ( 'NONE', #4525, #26924, #18175, .T. ) ;
#20648 = VERTEX_POINT ( 'NONE', #5086 ) ;
#20649 = ORIENTED_EDGE ( 'NONE', *, *, #22490, .F. ) ;
#20650 = VERTEX_POINT ( 'NONE', #13875 ) ;
#20651 = EDGE_LOOP ( 'NONE', ( #12209, #20680, #21172, #4285 ) ) ;
#20652 = CARTESIAN_POINT ( 'NONE',  ( -85.26706196341493182, 136.4560777204422948, 13.48389049418808661 ) ) ;
#20653 = DIRECTION ( 'NONE',  ( -0.5457381880580733924, -0.8379557447115514313, 0.000000000000000000 ) ) ;
#20654 = DIRECTION ( 'NONE',  ( -1.850371707708594316E-16, 1.000000000000000000, 0.000000000000000000 ) ) ;
#20655 = CARTESIAN_POINT ( 'NONE',  ( 124.3660254037843771, 240.4185842870417105, 45.00000000000000000 ) ) ;
#20656 = CARTESIAN_POINT ( 'NONE',  ( -73.01279441628793165, 126.4618695315959087, -45.00000000000000000 ) ) ;
#20657 = DIRECTION ( 'NONE',  ( -0.000000000000000000, -1.000000000000000000, -0.000000000000000000 ) ) ;
#20658 = CARTESIAN_POINT ( 'NONE',  ( 184.7759657584203694, 39.02219989801907474, -45.00000000000000000 ) ) ;
#20659 = LINE ( 'NONE', #13939, #18186 ) ;
#20660 = AXIS2_PLACEMENT_3D ( 'NONE', #8819, #59, #17579 ) ;
#20661 = CARTESIAN_POINT ( 'NONE',  ( 79.99999999999992895, 110.0000000000000000, -70.00000000000001421 ) ) ;
#20662 = CARTESIAN_POINT ( 'NONE',  ( -229.5850194865393519, 91.64208065330865338, -13.15559042349177687 ) ) ;
#20663 = DIRECTION ( 'NONE',  ( -0.000000000000000000, 1.000000000000000000, -0.000000000000000000 ) ) ;
#20664 = DIRECTION ( 'NONE',  ( -0.000000000000000000, -0.000000000000000000, -1.000000000000000000 ) ) ;
#20665 = VECTOR ( 'NONE', #18029, 1000.000000000000000 ) ;
#20666 = CARTESIAN_POINT ( 'NONE',  ( 65.00000000000000000, -120.0250000000000625, 70.00000000000001421 ) ) ;
#20667 = LINE ( 'NONE', #27401, #14766 ) ;
#20668 = EDGE_CURVE ( 'NONE', #20790, #14035, #649, .T. ) ;
#20669 = FACE_OUTER_BOUND ( 'NONE', #10731, .T. ) ;
#20671 = VERTEX_POINT ( 'NONE', #20602 ) ;
#20670 = ORIENTED_EDGE ( 'NONE', *, *, #25248, .T. ) ;
#20672 = EDGE_CURVE ( 'NONE', #15498, #16458, #7541, .T. ) ;
#20673 = EDGE_CURVE ( 'NONE', #19152, #7888, #26929, .T. ) ;
#20674 = CARTESIAN_POINT ( 'NONE',  ( 157.9999999999998863, 216.4921249924925348, 45.00000000000000000 ) ) ;
#20675 = EDGE_CURVE ( 'NONE', #12678, #21329, #25191, .T. ) ;
#20676 = VERTEX_POINT ( 'NONE', #1065 ) ;
#20677 = ORIENTED_EDGE ( 'NONE', *, *, #12709, .F. ) ;
#20678 = AXIS2_PLACEMENT_3D ( 'NONE', #18016, #13718, #20163 ) ;
#20679 = ORIENTED_EDGE ( 'NONE', *, *, #23476, .F. ) ;
#20680 = ORIENTED_EDGE ( 'NONE', *, *, #27843, .F. ) ;
#20681 = CARTESIAN_POINT ( 'NONE',  ( -79.00187704905532371, 96.44595867864549632, -155.7188177565815579 ) ) ;
#20682 = CARTESIAN_POINT ( 'NONE',  ( -528.3536063663644882, -163.3555848104747383, 0.000000000000000000 ) ) ;
#20683 = VECTOR ( 'NONE', #8869, 1000.000000000000114 ) ;
#20684 = CARTESIAN_POINT ( 'NONE',  ( 9.345921402568901470, 140.0000000000000000, 13.00000000000000000 ) ) ;
#20685 = CARTESIAN_POINT ( 'NONE',  ( 100.0424356845176135, 235.0879599625497463, -22.67299618748800327 ) ) ;
#20686 = FACE_OUTER_BOUND ( 'NONE', #1073, .T. ) ;
#20687 = LINE ( 'NONE', #18264, #20408 ) ;
#20688 = FACE_OUTER_BOUND ( 'NONE', #21980, .T. ) ;
#20689 = LINE ( 'NONE', #3581, #6552 ) ;
#20690 = ADVANCED_FACE ( 'NONE', ( #22628 ), #18956, .T. ) ;
#20691 = ADVANCED_FACE ( 'NONE', ( #22768 ), #22901, .F. ) ;
#20692 = AXIS2_PLACEMENT_3D ( 'NONE', #23383, #3693, #15773 ) ;
#20693 = CARTESIAN_POINT ( 'NONE',  ( 110.4531970035855579, 202.7493367244436513, -150.3892986974657617 ) ) ;
#20694 = LINE ( 'NONE', #21117, #13836 ) ;
#20695 = FACE_OUTER_BOUND ( 'NONE', #27339, .T. ) ;
#20696 = DIRECTION ( 'NONE',  ( 0.000000000000000000, -1.000000000000000000, 0.000000000000000000 ) ) ;
#20697 = ORIENTED_EDGE ( 'NONE', *, *, #3278, .T. ) ;
#20698 = FACE_OUTER_BOUND ( 'NONE', #9272, .T. ) ;
#20699 = EDGE_CURVE ( 'NONE', #22709, #9224, #787, .T. ) ;
#20700 = VECTOR ( 'NONE', #5466, 1000.000000000000000 ) ;
#20701 = ADVANCED_FACE ( 'NONE', ( #11996 ), #18728, .T. ) ;
#20702 = CARTESIAN_POINT ( 'NONE',  ( -232.3551040745953458, 65.57906652092701449, 15.97735746865810214 ) ) ;
#20703 = CARTESIAN_POINT ( 'NONE',  ( 154.4185842870419663, 232.3660254037841639, -45.00000000000000000 ) ) ;
#20704 = EDGE_LOOP ( 'NONE', ( #17320, #15031, #11482, #10458 ) ) ;
#20705 = DIRECTION ( 'NONE',  ( 0.000000000000000000, -1.000000000000000000, 1.387778780781445429E-16 ) ) ;
#20706 = EDGE_LOOP ( 'NONE', ( #18694, #25730, #2868, #6229 ) ) ;
#20707 = DIRECTION ( 'NONE',  ( -0.5975062131282562472, 0.8018642810807392607, 0.000000000000000000 ) ) ;
#20708 = LINE ( 'NONE', #21274, #11318 ) ;
#20709 = EDGE_LOOP ( 'NONE', ( #4139, #6865, #2116, #4506 ) ) ;
#20710 = ORIENTED_EDGE ( 'NONE', *, *, #9191, .F. ) ;
#20711 = DIRECTION ( 'NONE',  ( -0.000000000000000000, -0.000000000000000000, -1.000000000000000000 ) ) ;
#20712 = CIRCLE ( 'NONE', #28038, 30.00000000000000000 ) ;
#20713 = CARTESIAN_POINT ( 'NONE',  ( 217.4749999999996533, 258.6181251126050711, -5.999999999999991118 ) ) ;
#20714 = LINE ( 'NONE', #22743, #17840 ) ;
#20715 = ORIENTED_EDGE ( 'NONE', *, *, #3143, .F. ) ;
#20716 = CARTESIAN_POINT ( 'NONE',  ( 0.000000000000000000, -280.0000000000000000, 110.0000000000000284 ) ) ;
#20717 = ORIENTED_EDGE ( 'NONE', *, *, #5908, .T. ) ;
#20718 = AXIS2_PLACEMENT_3D ( 'NONE', #6927, #187, #15288 ) ;
#20719 = LINE ( 'NONE', #5492, #14820 ) ;
#20720 = AXIS2_PLACEMENT_3D ( 'NONE', #8732, #26250, #6576 ) ;
#20721 = LINE ( 'NONE', #487, #24108 ) ;
#20722 = CARTESIAN_POINT ( 'NONE',  ( 158.0000000000014779, 63.51174953456337136, -45.00000000000000000 ) ) ;
#20723 = EDGE_CURVE ( 'NONE', #18134, #7521, #27474, .T. ) ;
#20724 = DIRECTION ( 'NONE',  ( -1.000000000000000000, 0.000000000000000000, 0.000000000000000000 ) ) ;
#20725 = CYLINDRICAL_SURFACE ( 'NONE', #18297, 5.999999999999991118 ) ;
#20726 = DIRECTION ( 'NONE',  ( -0.8916010070293783896, -0.4528218681382319422, 0.000000000000000000 ) ) ;
#20727 = LINE ( 'NONE', #7667, #21671 ) ;
#20728 = EDGE_CURVE ( 'NONE', #7226, #14597, #3493, .T. ) ;
#20729 = ORIENTED_EDGE ( 'NONE', *, *, #20943, .F. ) ;
#20730 = FACE_BOUND ( 'NONE', #6389, .T. ) ;
#20731 = DIRECTION ( 'NONE',  ( 0.000000000000000000, -1.000000000000000000, 0.000000000000000000 ) ) ;
#20732 = DIRECTION ( 'NONE',  ( 1.000000000000000000, -0.000000000000000000, -0.000000000000000000 ) ) ;
#20733 = EDGE_LOOP ( 'NONE', ( #9773, #3208, #10184, #19115 ) ) ;
#20734 = DIRECTION ( 'NONE',  ( 0.000000000000000000, -1.000000000000000000, 0.000000000000000000 ) ) ;
#20735 = ORIENTED_EDGE ( 'NONE', *, *, #2655, .F. ) ;
#20736 = AXIS2_PLACEMENT_3D ( 'NONE', #3488, #10812, #13122 ) ;
#20737 = DIRECTION ( 'NONE',  ( 1.000000000000000000, 0.000000000000000000, 0.000000000000000000 ) ) ;
#20738 = CARTESIAN_POINT ( 'NONE',  ( -295.0000000000001137, -170.0000000000001137, 60.00000000000002842 ) ) ;
#20739 = CARTESIAN_POINT ( 'NONE',  ( 135.1960665634829581, 250.0000000000000568, -138.9999999999999432 ) ) ;
#20740 = VERTEX_POINT ( 'NONE', #3067 ) ;
#20741 = CARTESIAN_POINT ( 'NONE',  ( -175.0000000000000000, -150.0000000000000853, 70.00000000000001421 ) ) ;
#20742 = CARTESIAN_POINT ( 'NONE',  ( 158.0000000000009663, 115.6692496847042264, 45.00000000000000000 ) ) ;
#20743 = CIRCLE ( 'NONE', #27176, 5.999999999999991118 ) ;
#20744 = ORIENTED_EDGE ( 'NONE', *, *, #22102, .T. ) ;
#20745 =( GEOMETRIC_REPRESENTATION_CONTEXT ( 3 ) GLOBAL_UNCERTAINTY_ASSIGNED_CONTEXT ( ( #6591 ) ) GLOBAL_UNIT_ASSIGNED_CONTEXT ( ( #17884, #2080, #19613 ) ) REPRESENTATION_CONTEXT ( 'NONE', 'WORKASPACE' ) );
#20746 = EDGE_CURVE ( 'NONE', #19335, #17217, #15299, .T. ) ;
#20747 = DIRECTION ( 'NONE',  ( -0.8916010070296023216, -0.4528218681377911281, 0.000000000000000000 ) ) ;
#20748 = CARTESIAN_POINT ( 'NONE',  ( 109.5784832860911422, 255.7788523555518054, 37.68001940528806415 ) ) ;
#20749 = ORIENTED_EDGE ( 'NONE', *, *, #9503, .F. ) ;
#20750 = ORIENTED_EDGE ( 'NONE', *, *, #4436, .T. ) ;
#20751 = DIRECTION ( 'NONE',  ( -0.000000000000000000, -0.000000000000000000, -1.000000000000000000 ) ) ;
#20752 = ORIENTED_EDGE ( 'NONE', *, *, #27368, .F. ) ;
#20753 = EDGE_LOOP ( 'NONE', ( #17298, #7006, #5250, #11151 ) ) ;
#20754 = ORIENTED_EDGE ( 'NONE', *, *, #9786, .F. ) ;
#20755 = EDGE_CURVE ( 'NONE', #11099, #20391, #6120, .T. ) ;
#20756 = VECTOR ( 'NONE', #19944, 1000.000000000000000 ) ;
#20757 = LINE ( 'NONE', #14306, #22130 ) ;
#20758 = CONICAL_SURFACE ( 'NONE', #22132, 6.025000000000002132, 0.7853981633974482790 ) ;
#20759 = DIRECTION ( 'NONE',  ( 1.000000000000000000, 0.000000000000000000, 0.000000000000000000 ) ) ;
#20760 = CARTESIAN_POINT ( 'NONE',  ( -217.6530433929989101, 140.9974892713794645, -15.00000000000000000 ) ) ;
#20761 = AXIS2_PLACEMENT_3D ( 'NONE', #24266, #1851, #19673 ) ;
#20762 = EDGE_CURVE ( 'NONE', #24423, #21378, #17051, .T. ) ;
#20763 = AXIS2_PLACEMENT_3D ( 'NONE', #23189, #3498, #12284 ) ;
#20764 = CARTESIAN_POINT ( 'NONE',  ( 109.5756401952514523, 134.3783162855169451, -89.68749999975639753 ) ) ;
#20765 = FACE_OUTER_BOUND ( 'NONE', #257, .T. ) ;
#20766 = ADVANCED_FACE ( 'NONE', ( #10116 ), #155, .T. ) ;
#20767 = PLANE ( 'NONE',  #19839 ) ;
#20768 = PLANE ( 'NONE',  #25076 ) ;
#20769 = CARTESIAN_POINT ( 'NONE',  ( -260.0000000000001705, -167.0819201924624622, 110.0000000000000142 ) ) ;
#20770 = FACE_OUTER_BOUND ( 'NONE', #26077, .T. ) ;
#20771 = DIRECTION ( 'NONE',  ( 0.8916010070294402290, 0.4528218681381102617, 0.000000000000000000 ) ) ;
#20772 = ORIENTED_EDGE ( 'NONE', *, *, #11870, .F. ) ;
#20773 = CARTESIAN_POINT ( 'NONE',  ( 106.1556986643225002, 248.1950218616640598, -24.28466094498536165 ) ) ;
#20774 = LINE ( 'NONE', #20918, #26353 ) ;
#20775 = SURFACE_STYLE_USAGE ( .BOTH. , #25510 ) ;
#20776 = DIRECTION ( 'NONE',  ( 0.000000000000000000, 0.000000000000000000, -1.000000000000000000 ) ) ;
#20777 = ORIENTED_EDGE ( 'NONE', *, *, #3674, .F. ) ;
#20778 = AXIS2_PLACEMENT_3D ( 'NONE', #13005, #12858, #21754 ) ;
#20779 = EDGE_CURVE ( 'NONE', #855, #4042, #19290, .T. ) ;
#20780 = ADVANCED_FACE ( 'NONE', ( #18865 ), #6573, .F. ) ;
#20781 = AXIS2_PLACEMENT_3D ( 'NONE', #15953, #2571, #7035 ) ;
#20782 = CARTESIAN_POINT ( 'NONE',  ( 157.4999999999998579, 123.4468122109788482, -45.00000000000000000 ) ) ;
#20783 = ORIENTED_EDGE ( 'NONE', *, *, #3451, .F. ) ;
#20784 = DIRECTION ( 'NONE',  ( -0.7730186417261847298, -0.6343833064826063239, 0.000000000000000000 ) ) ;
#20785 = ORIENTED_EDGE ( 'NONE', *, *, #28127, .T. ) ;
#20786 = CIRCLE ( 'NONE', #10700, 5.999999999999991118 ) ;
#20787 = ORIENTED_EDGE ( 'NONE', *, *, #866, .F. ) ;
#20788 = VECTOR ( 'NONE', #20747, 1000.000000000000000 ) ;
#20789 = EDGE_LOOP ( 'NONE', ( #121, #4728, #9878, #11319, #27714, #8740 ) ) ;
#20790 = VERTEX_POINT ( 'NONE', #1621 ) ;
#20791 = VERTEX_POINT ( 'NONE', #27615 ) ;
#20792 = DIRECTION ( 'NONE',  ( 1.000000000000000000, 0.000000000000000000, 0.000000000000000000 ) ) ;
#20793 = ADVANCED_FACE ( 'NONE', ( #25745 ), #6352, .F. ) ;
#20794 = CARTESIAN_POINT ( 'NONE',  ( 167.4999999999996589, 258.6181251126050711, 6.000000000000019540 ) ) ;
#20795 = CARTESIAN_POINT ( 'NONE',  ( -210.6507024897083795, -220.0000000000000853, -91.36902465222451042 ) ) ;
#20796 = DIRECTION ( 'NONE',  ( -0.000000000000000000, -0.000000000000000000, -1.000000000000000000 ) ) ;
#20797 = ADVANCED_FACE ( 'NONE', ( #19146 ), #27756, .F. ) ;
#20798 = DIRECTION ( 'NONE',  ( 0.000000000000000000, 1.000000000000000000, -0.000000000000000000 ) ) ;
#20799 = AXIS2_PLACEMENT_3D ( 'NONE', #2302, #6907, #23 ) ;
#20800 = EDGE_CURVE ( 'NONE', #11282, #4619, #16993, .T. ) ;
#20801 = CARTESIAN_POINT ( 'NONE',  ( -196.2821818994568162, 62.43869624199520985, 34.70549414534111321 ) ) ;
#20802 = CARTESIAN_POINT ( 'NONE',  ( 158.0000000000001421, 193.4133749174225443, -45.00000000000000000 ) ) ;
#20803 = CARTESIAN_POINT ( 'NONE',  ( -77.52393792358382996, 136.3037775726609482, -13.50824672331413723 ) ) ;
#20804 = VECTOR ( 'NONE', #2317, 1000.000000000000000 ) ;
#20805 = CYLINDRICAL_SURFACE ( 'NONE', #16792, 22.49999999999999289 ) ;
#20806 = FACE_OUTER_BOUND ( 'NONE', #13308, .T. ) ;
#20807 = EDGE_CURVE ( 'NONE', #2640, #22383, #27892, .T. ) ;
#20808 = AXIS2_PLACEMENT_3D ( 'NONE', #20170, #7248, #11129 ) ;
#20809 = DIRECTION ( 'NONE',  ( 0.000000000000000000, 0.000000000000000000, -1.000000000000000000 ) ) ;
#20810 = PLANE ( 'NONE',  #10011 ) ;
#20811 = CARTESIAN_POINT ( 'NONE',  ( 158.0000000000002558, 181.3818748873943889, 45.00000000000000000 ) ) ;
#20812 = ORIENTED_EDGE ( 'NONE', *, *, #23582, .T. ) ;
#20813 = FACE_OUTER_BOUND ( 'NONE', #2528, .T. ) ;
#20814 = CARTESIAN_POINT ( 'NONE',  ( 106.3487426207649236, 91.82653269718771583, -100.0000000000000142 ) ) ;
#20815 = CARTESIAN_POINT ( 'NONE',  ( 157.4999999999998579, 201.1909374436971802, -45.00000000000000000 ) ) ;
#20817 = ORIENTED_EDGE ( 'NONE', *, *, #12160, .F. ) ;
#20816 = VERTEX_POINT ( 'NONE', #7954 ) ;
#20818 = CARTESIAN_POINT ( 'NONE',  ( 79.99999999999992895, 110.0000000000000000, 45.00000000000000000 ) ) ;
#20819 = ORIENTED_EDGE ( 'NONE', *, *, #21127, .T. ) ;
#20820 = ORIENTED_EDGE ( 'NONE', *, *, #11348, .T. ) ;
#20821 = EDGE_CURVE ( 'NONE', #21780, #2305, #16721, .T. ) ;
#20822 = AXIS2_PLACEMENT_3D ( 'NONE', #21605, #20798, #10554 ) ;
#20823 = VERTEX_POINT ( 'NONE', #28032 ) ;
#20824 = EDGE_LOOP ( 'NONE', ( #1310, #20280, #24791, #3856 ) ) ;
#20825 = VECTOR ( 'NONE', #5366, 1000.000000000000000 ) ;
#20826 = ORIENTED_EDGE ( 'NONE', *, *, #15521, .F. ) ;
#20827 = CARTESIAN_POINT ( 'NONE',  ( 157.9999999999996305, 286.7126252026890256, 45.00000000000000000 ) ) ;
#20828 = CARTESIAN_POINT ( 'NONE',  ( 157.4999999999998010, 241.3169375638095460, -45.00000000000000000 ) ) ;
#20829 = LINE ( 'NONE', #9921, #9634 ) ;
#20830 = CARTESIAN_POINT ( 'NONE',  ( 101.0134753670012913, 235.9904216347473778, -23.57078716685460407 ) ) ;
#20831 = ADVANCED_FACE ( 'NONE', ( #1895 ), #25474, .F. ) ;
#20832 = EDGE_CURVE ( 'NONE', #6513, #6126, #3914, .T. ) ;
#20833 = CARTESIAN_POINT ( 'NONE',  ( -71.37541315349507443, 150.2892445414773590, -15.00000000000000000 ) ) ;
#20834 = LINE ( 'NONE', #1153, #7585 ) ;
#20835 = CARTESIAN_POINT ( 'NONE',  ( 157.9999999999996589, 278.6811251726610976, 45.00000000000000000 ) ) ;
#20836 = CARTESIAN_POINT ( 'NONE',  ( 158.0000000000007958, 128.7164997297464595, -45.00000000000000000 ) ) ;
#20837 = VECTOR ( 'NONE', #26466, 1000.000000000000000 ) ;
#20838 = DIRECTION ( 'NONE',  ( -0.000000000000000000, -4.625929269271485914E-16, 1.000000000000000000 ) ) ;
#20839 = DIRECTION ( 'NONE',  ( -1.000000000000000000, 0.000000000000000000, 0.000000000000000000 ) ) ;
#20840 = CARTESIAN_POINT ( 'NONE',  ( 158.0000000000012506, 86.08262460212675649, 45.00000000000000000 ) ) ;
#20841 = CIRCLE ( 'NONE', #24501, 5.999999999999991118 ) ;
#20842 = CARTESIAN_POINT ( 'NONE',  ( 158.0000000000000284, 203.9527499549551806, 45.00000000000000000 ) ) ;
#20843 = ORIENTED_EDGE ( 'NONE', *, *, #14849, .T. ) ;
#20844 = CARTESIAN_POINT ( 'NONE',  ( -230.8916957670046486, 130.8330661503598833, 15.00000000000000000 ) ) ;
#20845 = EDGE_CURVE ( 'NONE', #2835, #26591, #2310, .T. ) ;
#20846 = DIRECTION ( 'NONE',  ( -0.9611633748070274041, -0.2759800118297804916, 1.182005470438334537E-13 ) ) ;
#20847 = ORIENTED_EDGE ( 'NONE', *, *, #27423, .T. ) ;
#20848 = CARTESIAN_POINT ( 'NONE',  ( 0.000000000000000000, 0.000000000000000000, 0.000000000000000000 ) ) ;
#20849 = ORIENTED_EDGE ( 'NONE', *, *, #20582, .T. ) ;
#20850 = ORIENTED_EDGE ( 'NONE', *, *, #14203, .F. ) ;
#20851 = CARTESIAN_POINT ( 'NONE',  ( 187.4999999999996305, 83.06687458711267880, -36.86484227207694175 ) ) ;
#20852 = EDGE_CURVE ( 'NONE', #22331, #3239, #1523, .T. ) ;
#20853 = LINE ( 'NONE', #14120, #14512 ) ;
#20854 = ORIENTED_EDGE ( 'NONE', *, *, #28211, .F. ) ;
#20855 = AXIS2_PLACEMENT_3D ( 'NONE', #12657, #19384, #25845 ) ;
#20856 = ORIENTED_EDGE ( 'NONE', *, *, #2323, .F. ) ;
#20857 = DIRECTION ( 'NONE',  ( 0.000000000000000000, 0.000000000000000000, -1.000000000000000000 ) ) ;
#20858 = DIRECTION ( 'NONE',  ( -0.3102637045530707294, -0.9506505318133497973, 0.000000000000000000 ) ) ;
#20859 = CARTESIAN_POINT ( 'NONE',  ( -15.28840184913744515, 9.956927649352207865, 45.00000000000000000 ) ) ;
#20860 = ORIENTED_EDGE ( 'NONE', *, *, #11520, .F. ) ;
#20861 = EDGE_CURVE ( 'NONE', #23826, #11334, #17416, .T. ) ;
#20862 = CARTESIAN_POINT ( 'NONE',  ( -230.9048883912569181, 92.57784203868951067, 15.03157938458457998 ) ) ;
#20863 = EDGE_LOOP ( 'NONE', ( #402, #24860, #1408, #15849 ) ) ;
#20864 = VECTOR ( 'NONE', #14322, 1000.000000000000114 ) ;
#20865 = LINE ( 'NONE', #23022, #17106 ) ;
#20866 = EDGE_CURVE ( 'NONE', #17812, #5015, #13263, .T. ) ;
#20867 = ADVANCED_FACE ( 'NONE', ( #2179 ), #26316, .F. ) ;
#20868 = CARTESIAN_POINT ( 'NONE',  ( 158.0000000000010516, 103.6377496546760568, 45.00000000000000000 ) ) ;
#20869 = DIRECTION ( 'NONE',  ( -0.4999999999999985012, 0.8660254037844394848, 0.000000000000000000 ) ) ;
#20870 = DIRECTION ( 'NONE',  ( -0.000000000000000000, -0.000000000000000000, -1.000000000000000000 ) ) ;
#20871 = CARTESIAN_POINT ( 'NONE',  ( 157.4999999999998295, 228.7775625262745223, 45.00000000000000000 ) ) ;
#20872 = CARTESIAN_POINT ( 'NONE',  ( 192.5108452903457419, 172.8810361401565672, 45.00000000000000000 ) ) ;
#20873 = CARTESIAN_POINT ( 'NONE',  ( -184.0582905406964471, 107.1919238267117720, -32.00588097399845111 ) ) ;
#20874 = VERTEX_POINT ( 'NONE', #6775 ) ;
#20875 = DIRECTION ( 'NONE',  ( -0.8916010070298462376, -0.4528218681373109011, 0.000000000000000000 ) ) ;
#20876 = CIRCLE ( 'NONE', #6644, 5.999999999999977796 ) ;
#20877 = LINE ( 'NONE', #25598, #13354 ) ;
#20878 = DIRECTION ( 'NONE',  ( 0.4528218681383106015, -0.8916010070293384215, 0.000000000000000000 ) ) ;
#20879 = LINE ( 'NONE', #16576, #5676 ) ;
#20880 = ORIENTED_EDGE ( 'NONE', *, *, #9784, .F. ) ;
#20881 = VECTOR ( 'NONE', #21344, 1000.000000000000000 ) ;
#20882 = DIRECTION ( 'NONE',  ( 0.8916010070293510781, -0.4528218681382856770, 0.000000000000000000 ) ) ;
#20883 = ORIENTED_EDGE ( 'NONE', *, *, #27961, .F. ) ;
#20884 = DIRECTION ( 'NONE',  ( 0.8916010070293383105, -0.4528218681383106015, 0.000000000000000000 ) ) ;
#20885 = CARTESIAN_POINT ( 'NONE',  ( -175.0000000000000000, -120.0000000000001847, -63.97499999999998721 ) ) ;
#20886 = DIRECTION ( 'NONE',  ( -0.8916010070296838119, -0.4528218681376305899, 0.000000000000000000 ) ) ;
#20887 = ORIENTED_EDGE ( 'NONE', *, *, #20151, .F. ) ;
#20888 = CARTESIAN_POINT ( 'NONE',  ( 158.0000000000002274, 183.8897498949014278, 45.00000000000000000 ) ) ;
#20889 = AXIS2_PLACEMENT_3D ( 'NONE', #22481, #24783, #218 ) ;
#20890 = ORIENTED_EDGE ( 'NONE', *, *, #14447, .F. ) ;
#20891 = PLANE ( 'NONE',  #2420 ) ;
#20892 = CARTESIAN_POINT ( 'NONE',  ( 199.9999999999998863, 0.000000000000000000, 110.0000000000000284 ) ) ;
#20893 = VERTEX_POINT ( 'NONE', #15558 ) ;
#20894 = ORIENTED_EDGE ( 'NONE', *, *, #900, .T. ) ;
#20895 = LINE ( 'NONE', #5807, #18208 ) ;
#20896 = ORIENTED_EDGE ( 'NONE', *, *, #27460, .T. ) ;
#20897 = EDGE_CURVE ( 'NONE', #24116, #27097, #22009, .T. ) ;
#20898 = VECTOR ( 'NONE', #10836, 1000.000000000000000 ) ;
#20899 = ORIENTED_EDGE ( 'NONE', *, *, #13450, .F. ) ;
#20900 = ORIENTED_EDGE ( 'NONE', *, *, #11461, .T. ) ;
#20901 = VECTOR ( 'NONE', #15772, 1000.000000000000114 ) ;
#20902 = LINE ( 'NONE', #24939, #3791 ) ;
#20903 = EDGE_CURVE ( 'NONE', #23690, #4054, #6641, .T. ) ;
#20904 = CARTESIAN_POINT ( 'NONE',  ( -180.0000000000000284, -40.00000000000004974, -70.00000000000001421 ) ) ;
#20905 = CARTESIAN_POINT ( 'NONE',  ( 158.0000000000003126, 178.3661248723802828, -45.00000000000000000 ) ) ;
#20906 = VECTOR ( 'NONE', #6518, 1000.000000000000000 ) ;
#20907 = CARTESIAN_POINT ( 'NONE',  ( -112.3221550338875687, 69.54464929955099706, 80.00000000000001421 ) ) ;
#20908 = CARTESIAN_POINT ( 'NONE',  ( 158.0000000000016769, 47.95662448201407102, 45.00000000000000000 ) ) ;
#20909 = CARTESIAN_POINT ( 'NONE',  ( 158.0000000000016769, 45.95662448201407102, 45.00000000000000000 ) ) ;
#20910 = EDGE_CURVE ( 'NONE', #7297, #25488, #15779, .T. ) ;
#20911 = CARTESIAN_POINT ( 'NONE',  ( 367.4999999999996021, 44.41075299063184900, 1.850330238640837654E-14 ) ) ;
#20912 = CARTESIAN_POINT ( 'NONE',  ( -274.6409284829297803, -170.0000000000001421, 102.7220467394344894 ) ) ;
#20913 = DIRECTION ( 'NONE',  ( -1.000000000000000000, 0.000000000000000000, 0.000000000000000000 ) ) ;
#20914 = CARTESIAN_POINT ( 'NONE',  ( -210.0000000000000000, -120.0000000000001705, 100.0000000000000142 ) ) ;
#20915 = VERTEX_POINT ( 'NONE', #10957 ) ;
#20916 = CARTESIAN_POINT ( 'NONE',  ( -11.61682370180709079, 131.4608765202114853, 14.74855702008673397 ) ) ;
#20917 = CARTESIAN_POINT ( 'NONE',  ( 91.94651231017051884, 240.0740382701074225, -7.116185459647595302 ) ) ;
#20918 = CARTESIAN_POINT ( 'NONE',  ( 158.0000000000003126, 178.3661248723802828, 45.00000000000000000 ) ) ;
#20919 = AXIS2_PLACEMENT_3D ( 'NONE', #16705, #25318, #1047 ) ;
#20920 = LINE ( 'NONE', #5970, #10472 ) ;
#20921 = DIRECTION ( 'NONE',  ( -1.000000000000000000, -0.000000000000000000, -0.000000000000000000 ) ) ;
#20922 = ORIENTED_EDGE ( 'NONE', *, *, #20942, .T. ) ;
#20923 = VECTOR ( 'NONE', #21485, 1000.000000000000000 ) ;
#20924 = CARTESIAN_POINT ( 'NONE',  ( -260.0000000000001137, -220.0000000000000853, -59.99999999999986500 ) ) ;
#20925 = ORIENTED_EDGE ( 'NONE', *, *, #20355, .T. ) ;
#20926 = CARTESIAN_POINT ( 'NONE',  ( 157.4999999999998579, 73.28931206083800021, 45.00000000000000000 ) ) ;
#20927 = ORIENTED_EDGE ( 'NONE', *, *, #894, .T. ) ;
#20928 =( BOUNDED_SURFACE ( )  B_SPLINE_SURFACE ( 2, 3, ( 
 ( #9945, #25305, #27312, #23157, #27446, #7788, #14403, #12255, #6757, #10796, #8921, #13242, #6477, #21710, #23720, #21560, #28011, #25869, #26007, #1733, #10936, #21418 ),
 ( #12957, #21987, #10508, #8354, #4029, #2295, #17114, #13109, #19555, #15400, #160, #6194, #2021, #6620, #6329, #28295, #15256, #21855, #19266, #15111, #12817, #8639 ),
 ( #3891, #10650, #11077, #17392, #2159, #14970, #1871, #19410, #19834, #26297, #28155, #26153, #8497, #24011, #17252, #24156, #4454, #17678, #4171, #26430, #4318, #19693 ) ),
 .UNSPECIFIED., .F., .F., .T. ) 
 B_SPLINE_SURFACE_WITH_KNOTS ( ( 3, 3 ),
 ( 4, 2, 2, 2, 2, 2, 2, 2, 2, 2, 4 ),
 ( 0.000000000000000000, 1.000000000000000000 ),
 ( 0.000000000000000000, 0.004677071733467426211, 0.009354143466934852422, 0.01403121520040227777, 0.01870828693386970484, 0.02806243040080455553, 0.03741657386773940969, 0.04677071733467426384, 0.05612486080160911106, 0.06547900426854397216, 0.07483314773547881937 ),
 .UNSPECIFIED. ) 
 GEOMETRIC_REPRESENTATION_ITEM ( )  RATIONAL_B_SPLINE_SURFACE ( (
 ( 1.000000000000000000, 1.000000000000000000, 1.000000000000000000, 1.000000000000000000, 1.000000000000000000, 1.000000000000000000, 1.000000000000000000, 1.000000000000000000, 1.000000000000000000, 1.000000000000000000, 1.000000000000000000, 1.000000000000000000, 1.000000000000000000, 1.000000000000000000, 1.000000000000000000, 1.000000000000000000, 1.000000000000000000, 1.000000000000000000, 1.000000000000000000, 1.000000000000000000, 1.000000000000000000, 1.000000000000000000),
 ( 0.7071067811865475727, 0.7071067811865475727, 0.7071067811865476838, 0.7071067811865476838, 0.7071067811865473507, 0.7071067811865473507, 0.7071067811865473507, 0.7071067811865473507, 0.7071067811865474617, 0.7071067811865474617, 0.7071067811865476838, 0.7071067811865476838, 0.7071067811865477948, 0.7071067811865477948, 0.7071067811865473507, 0.7071067811865473507, 0.7071067811865475727, 0.7071067811865475727, 0.7071067811865475727, 0.7071067811865475727, 0.7071067811865484609, 0.7071067811865484609),
 ( 1.000000000000000000, 1.000000000000000000, 1.000000000000000000, 1.000000000000000000, 1.000000000000000000, 1.000000000000000000, 1.000000000000000000, 1.000000000000000000, 1.000000000000000000, 1.000000000000000000, 1.000000000000000000, 1.000000000000000000, 1.000000000000000000, 1.000000000000000000, 1.000000000000000000, 1.000000000000000000, 1.000000000000000000, 1.000000000000000000, 1.000000000000000000, 1.000000000000000000, 1.000000000000000000, 1.000000000000000000) ) ) 
 REPRESENTATION_ITEM ( '' )  SURFACE ( )  );
#20929 = VECTOR ( 'NONE', #1548, 1000.000000000000000 ) ;
#20930 = VERTEX_POINT ( 'NONE', #11097 ) ;
#20931 = EDGE_CURVE ( 'NONE', #11179, #18978, #19424, .T. ) ;
#20932 = ORIENTED_EDGE ( 'NONE', *, *, #10406, .F. ) ;
#20933 = ORIENTED_EDGE ( 'NONE', *, *, #12963, .T. ) ;
#20934 = DIRECTION ( 'NONE',  ( -1.321694076934710155E-16, 1.000000000000000000, 0.000000000000000000 ) ) ;
#20935 = CYLINDRICAL_SURFACE ( 'NONE', #2639, 5.000000000000004441 ) ;
#20936 = CARTESIAN_POINT ( 'NONE',  ( 157.4999999999997726, 248.8405625863305204, 45.00000000000000000 ) ) ;
#20937 = CARTESIAN_POINT ( 'NONE',  ( -157.8317677482887973, 120.6968079807819407, -22.00051853850753147 ) ) ;
#20938 = VECTOR ( 'NONE', #14966, 1000.000000000000000 ) ;
#20939 = CARTESIAN_POINT ( 'NONE',  ( 158.0000000000014779, 63.51174953456337136, -45.00000000000000000 ) ) ;
#20940 = LINE ( 'NONE', #979, #10949 ) ;
#20941 = CARTESIAN_POINT ( 'NONE',  ( -156.3854698478411649, 122.2179277774955466, -19.69657316895759536 ) ) ;
#20942 = EDGE_CURVE ( 'NONE', #9382, #7691, #10818, .T. ) ;
#20943 = EDGE_CURVE ( 'NONE', #4251, #6860, #9229, .T. ) ;
#20944 = CARTESIAN_POINT ( 'NONE',  ( -24.92338318254761020, 127.6681916698425567, -145.0000000000000000 ) ) ;
#20945 = CARTESIAN_POINT ( 'NONE',  ( -212.2904188450821152, 87.25517758443818650, 23.57528053420220360 ) ) ;
#20946 = AXIS2_PLACEMENT_3D ( 'NONE', #16607, #12447, #7980 ) ;
#20947 = DIRECTION ( 'NONE',  ( 0.8916010070294904111, -0.4528218681380115074, 0.000000000000000000 ) ) ;
#20948 = CARTESIAN_POINT ( 'NONE',  ( 432.4999999999996589, -5.589247009368160768, 100.0000000000000426 ) ) ;
#20949 = CARTESIAN_POINT ( 'NONE',  ( 157.4999999999998579, 113.4153121809506786, -45.00000000000000000 ) ) ;
#20950 = ORIENTED_EDGE ( 'NONE', *, *, #28296, .T. ) ;
#20951 = CARTESIAN_POINT ( 'NONE',  ( -38.27121137906592452, -18.98690351477092619, 99.90775530369607793 ) ) ;
#20952 = CARTESIAN_POINT ( 'NONE',  ( 100.8904249506145874, 86.57652225509636423, -100.0000000000000142 ) ) ;
#20953 = CARTESIAN_POINT ( 'NONE',  ( 157.9999999999998295, 226.0157500150140208, 45.00000000000000000 ) ) ;
#20955 = EDGE_LOOP ( 'NONE', ( #12037, #19651, #27935, #10758 ) ) ;
#20954 = ORIENTED_EDGE ( 'NONE', *, *, #13619, .F. ) ;
#20956 = EDGE_CURVE ( 'NONE', #16518, #25350, #8795, .T. ) ;
#20957 = EDGE_CURVE ( 'NONE', #25380, #17988, #21871, .T. ) ;
#20958 = CARTESIAN_POINT ( 'NONE',  ( 141.9187638636469160, 241.9574749595457774, 45.00000000000000000 ) ) ;
#20959 = EDGE_LOOP ( 'NONE', ( #363, #4512, #4690, #19620 ) ) ;
#20960 = ORIENTED_EDGE ( 'NONE', *, *, #12141, .F. ) ;
#20961 = AXIS2_PLACEMENT_3D ( 'NONE', #18878, #23473, #3787 ) ;
#20962 = ORIENTED_EDGE ( 'NONE', *, *, #25091, .F. ) ;
#20963 = ORIENTED_EDGE ( 'NONE', *, *, #2154, .T. ) ;
#20964 = EDGE_CURVE ( 'NONE', #477, #22143, #15421, .T. ) ;
#20965 = ORIENTED_EDGE ( 'NONE', *, *, #3638, .F. ) ;
#20966 = VERTEX_POINT ( 'NONE', #13547 ) ;
#20967 = FACE_OUTER_BOUND ( 'NONE', #27977, .T. ) ;
#20968 = FACE_OUTER_BOUND ( 'NONE', #13992, .T. ) ;
#20969 = PLANE ( 'NONE',  #19421 ) ;
#20970 = CARTESIAN_POINT ( 'NONE',  ( 1.554977376564339764, 135.1207837442669870, -15.37741204235645931 ) ) ;
#20971 = DIRECTION ( 'NONE',  ( 1.850371707708594316E-16, -1.000000000000000000, -0.000000000000000000 ) ) ;
#20972 = CARTESIAN_POINT ( 'NONE',  ( 157.4999999999998579, 60.74993702330277756, 45.00000000000000000 ) ) ;
#20973 = CARTESIAN_POINT ( 'NONE',  ( -194.2306746384193730, 63.21821459927384979, -44.70951427402087575 ) ) ;
#20974 = VECTOR ( 'NONE', #698, 1000.000000000000000 ) ;
#20975 = DIRECTION ( 'NONE',  ( 1.000000000000000000, -0.000000000000000000, 0.000000000000000000 ) ) ;
#20976 = CARTESIAN_POINT ( 'NONE',  ( 158.0000000000011653, 95.60624962464788723, 45.00000000000000000 ) ) ;
#20977 = CARTESIAN_POINT ( 'NONE',  ( 156.5461074670752453, 207.5603490538953224, -145.0000000000000000 ) ) ;
#20978 = CARTESIAN_POINT ( 'NONE',  ( 157.4999999999998579, 100.8759371434154701, 45.00000000000000000 ) ) ;
#20979 = ORIENTED_EDGE ( 'NONE', *, *, #708, .T. ) ;
#20980 = DIRECTION ( 'NONE',  ( 0.5241030343220994814, 0.8516548651973804285, -0.000000000000000000 ) ) ;
#20981 = LINE ( 'NONE', #25023, #23190 ) ;
#20982 = ORIENTED_EDGE ( 'NONE', *, *, #2120, .F. ) ;
#20983 = CARTESIAN_POINT ( 'NONE',  ( 0.000000000000000000, 0.000000000000000000, 0.000000000000000000 ) ) ;
#20984 = ORIENTED_EDGE ( 'NONE', *, *, #5867, .T. ) ;
#20986 = ADVANCED_FACE ( 'NONE', ( #327 ), #11391, .F. ) ;
#20985 = EDGE_LOOP ( 'NONE', ( #19578, #27007, #11898, #11331 ) ) ;
#20987 = VECTOR ( 'NONE', #3196, 1000.000000000000000 ) ;
#20988 = CARTESIAN_POINT ( 'NONE',  ( 93.07270601806959576, 112.9533406969986231, 99.99999999997838529 ) ) ;
#20989 = DIRECTION ( 'NONE',  ( -0.000000000000000000, -0.000000000000000000, -1.000000000000000000 ) ) ;
#20990 = EDGE_LOOP ( 'NONE', ( #6221, #17912, #3608, #1042 ) ) ;
#20991 = ORIENTED_EDGE ( 'NONE', *, *, #9177, .F. ) ;
#20992 = LINE ( 'NONE', #10087, #14548 ) ;
#20993 = CARTESIAN_POINT ( 'NONE',  ( 109.9999999999999432, 259.1952685963541967, 44.30308214094263519 ) ) ;
#20994 = LINE ( 'NONE', #23016, #21061 ) ;
#20995 = ORIENTED_EDGE ( 'NONE', *, *, #18284, .F. ) ;
#20996 = CARTESIAN_POINT ( 'NONE',  ( -277.2150368962633706, -165.0000000000001137, 101.5769467933889416 ) ) ;
#20997 = ORIENTED_EDGE ( 'NONE', *, *, #20755, .T. ) ;
#20998 = DIRECTION ( 'NONE',  ( -1.000000000000000000, 0.000000000000000000, 0.000000000000000000 ) ) ;
#20999 = DIRECTION ( 'NONE',  ( -1.000000000000000000, 6.167905692361982533E-16, 0.000000000000000000 ) ) ;
#21000 = CARTESIAN_POINT ( 'NONE',  ( 158.0000000000006253, 146.2716247822957598, 45.00000000000000000 ) ) ;
#21001 = CARTESIAN_POINT ( 'NONE',  ( 187.4999999999996305, 83.06687458711267880, 30.86484227207694886 ) ) ;
#21002 = DIRECTION ( 'NONE',  ( 0.4528218681379702626, -0.8916010070295112833, 0.000000000000000000 ) ) ;
#21003 = DIRECTION ( 'NONE',  ( 2.220446049250266932E-15, 0.000000000000000000, -1.000000000000000000 ) ) ;
#21004 = CARTESIAN_POINT ( 'NONE',  ( 163.0331409777209331, 209.3154830203752397, -148.6534330424975963 ) ) ;
#21005 = VECTOR ( 'NONE', #12344, 1000.000000000000000 ) ;
#21006 = ORIENTED_EDGE ( 'NONE', *, *, #13788, .T. ) ;
#21007 = EDGE_CURVE ( 'NONE', #7044, #17060, #26307, .T. ) ;
#21008 = DIRECTION ( 'NONE',  ( 0.4528218681371922183, 0.8916010070299064116, -0.000000000000000000 ) ) ;
#21009 = VECTOR ( 'NONE', #4929, 1000.000000000000000 ) ;
#21010 = CARTESIAN_POINT ( 'NONE',  ( -180.0000000000000284, -40.00000000000004974, 100.0000000000000142 ) ) ;
#21011 = CYLINDRICAL_SURFACE ( 'NONE', #6050, 7.499999999999992895 ) ;
#21012 = LINE ( 'NONE', #16301, #20825 ) ;
#21013 = ORIENTED_EDGE ( 'NONE', *, *, #4124, .T. ) ;
#21014 = LINE ( 'NONE', #4049, #22900 ) ;
#21015 = ORIENTED_EDGE ( 'NONE', *, *, #6659, .T. ) ;
#21016 = CARTESIAN_POINT ( 'NONE',  ( -189.7025054116240881, 103.6028096261271259, 32.02907974114463485 ) ) ;
#21017 = FACE_OUTER_BOUND ( 'NONE', #9463, .T. ) ;
#21018 = DIRECTION ( 'NONE',  ( 1.000000000000000000, -0.000000000000000000, -0.000000000000000000 ) ) ;
#21019 = ORIENTED_EDGE ( 'NONE', *, *, #22662, .T. ) ;
#21020 = DIRECTION ( 'NONE',  ( 0.8916010070293584056, -0.4528218681382712996, 0.000000000000000000 ) ) ;
#21021 = DIRECTION ( 'NONE',  ( 0.000000000000000000, 0.000000000000000000, -1.000000000000000000 ) ) ;
#21022 = EDGE_CURVE ( 'NONE', #5376, #20790, #20137, .T. ) ;
#21023 = EDGE_LOOP ( 'NONE', ( #25304, #23392, #15676, #16206 ) ) ;
#21024 = EDGE_CURVE ( 'NONE', #1063, #7087, #22592, .T. ) ;
#21025 = EDGE_CURVE ( 'NONE', #22340, #1342, #26894, .T. ) ;
#21026 = DIRECTION ( 'NONE',  ( 0.000000000000000000, 1.000000000000000000, 1.214306433183764966E-16 ) ) ;
#21027 = ADVANCED_FACE ( 'NONE', ( #616 ), #9380, .F. ) ;
#21028 = DIRECTION ( 'NONE',  ( 0.000000000000000000, -1.000000000000000000, 0.000000000000000000 ) ) ;
#21029 = ORIENTED_EDGE ( 'NONE', *, *, #10623, .F. ) ;
#21030 = ORIENTED_EDGE ( 'NONE', *, *, #16904, .T. ) ;
#21031 = DIRECTION ( 'NONE',  ( 0.4528218681376106058, -0.8916010070296940260, 0.000000000000000000 ) ) ;
#21032 = ORIENTED_EDGE ( 'NONE', *, *, #22693, .T. ) ;
#21033 = CIRCLE ( 'NONE', #1304, 2.000000000000000000 ) ;
#21034 = PRODUCT_DEFINITION_SHAPE ( 'NONE', 'NONE',  #20363 ) ;
#21035 = VECTOR ( 'NONE', #3687, 1000.000000000000000 ) ;
#21036 = ORIENTED_EDGE ( 'NONE', *, *, #13251, .T. ) ;
#21037 = ORIENTED_EDGE ( 'NONE', *, *, #25248, .F. ) ;
#21038 = CARTESIAN_POINT ( 'NONE',  ( 109.9999999999459703, 259.2933449746407746, 44.14322629295149625 ) ) ;
#21039 = CARTESIAN_POINT ( 'NONE',  ( -210.0000000000000853, -218.4793454996984394, 109.3807997302053963 ) ) ;
#21040 = LINE ( 'NONE', #14730, #25679 ) ;
#21041 = DIRECTION ( 'NONE',  ( -0.000000000000000000, -0.000000000000000000, -1.000000000000000000 ) ) ;
#21042 = DIRECTION ( 'NONE',  ( 1.000000000000000000, 0.000000000000000000, 0.000000000000000000 ) ) ;
#21043 = CARTESIAN_POINT ( 'NONE',  ( 232.4999999999996305, 133.0668745871126930, -36.86484227207694886 ) ) ;
#21044 = VECTOR ( 'NONE', #20128, 1000.000000000000000 ) ;
#21045 = DIRECTION ( 'NONE',  ( 0.000000000000000000, 0.000000000000000000, -1.000000000000000000 ) ) ;
#21046 = B_SPLINE_CURVE_WITH_KNOTS ( 'NONE', 3,
 ( #11173, #21943, #20066, #17633, #21807, #18069 ),
 .UNSPECIFIED., .F., .F.,
 ( 4, 2, 4 ),
 ( 0.0003697107221120765510, 0.0006673033929023622877, 0.0009648960636926479702 ),
 .UNSPECIFIED. ) ;
#21047 = CARTESIAN_POINT ( 'NONE',  ( 157.4999999999998579, 80.81293708335913095, 45.00000000000000000 ) ) ;
#21048 = CARTESIAN_POINT ( 'NONE',  ( 0.2662533044063318810, -1.249999999999998890, -7.393438799766935965 ) ) ;
#21049 = CARTESIAN_POINT ( 'NONE',  ( 158.0000000000001990, 186.3976249024084666, 45.00000000000000000 ) ) ;
#21050 = ORIENTED_EDGE ( 'NONE', *, *, #3205, .F. ) ;
#21051 = LINE ( 'NONE', #1655, #17370 ) ;
#21052 = EDGE_CURVE ( 'NONE', #8056, #25897, #886, .T. ) ;
#21053 = AXIS2_PLACEMENT_3D ( 'NONE', #1786, #28208, #13019 ) ;
#21054 = ADVANCED_FACE ( 'NONE', ( #27299 ), #24745, .F. ) ;
#21055 = AXIS2_PLACEMENT_3D ( 'NONE', #18963, #3721, #27563 ) ;
#21056 = CARTESIAN_POINT ( 'NONE',  ( 106.4996638054810489, 248.6817669671922317, -25.16380096945068345 ) ) ;
#21057 = CARTESIAN_POINT ( 'NONE',  ( -140.1240808061633345, 61.15703788601678781, 393.1631314933625845 ) ) ;
#21058 = DIRECTION ( 'NONE',  ( -1.000000000000000000, 0.000000000000000000, 0.000000000000000000 ) ) ;
#21059 = CARTESIAN_POINT ( 'NONE',  ( 115.5814157129579058, 207.6339745962153245, -45.00000000000000000 ) ) ;
#21060 = ORIENTED_EDGE ( 'NONE', *, *, #9358, .T. ) ;
#21061 = VECTOR ( 'NONE', #9671, 1000.000000000000000 ) ;
#21062 = CARTESIAN_POINT ( 'NONE',  ( 73.69623568533953062, -15.56365422765611051, -45.00000000000000000 ) ) ;
#21063 = ORIENTED_EDGE ( 'NONE', *, *, #12775, .F. ) ;
#21064 = ADVANCED_FACE ( 'NONE', ( #9660 ), #10107, .T. ) ;
#21065 = FACE_OUTER_BOUND ( 'NONE', #25766, .T. ) ;
#21066 = ORIENTED_EDGE ( 'NONE', *, *, #4448, .T. ) ;
#21067 = VERTEX_POINT ( 'NONE', #3122 ) ;
#21068 = CARTESIAN_POINT ( 'NONE',  ( -82.72863776448107842, 136.4212039060443828, 15.16706508184716462 ) ) ;
#21069 = VECTOR ( 'NONE', #20734, 1000.000000000000000 ) ;
#21070 = CIRCLE ( 'NONE', #28391, 41.00000000000000711 ) ;
#21071 = ORIENTED_EDGE ( 'NONE', *, *, #10364, .F. ) ;
#21072 = ORIENTED_EDGE ( 'NONE', *, *, #3680, .T. ) ;
#21073 = CARTESIAN_POINT ( 'NONE',  ( 134.9999999999998579, 244.8793018922092699, -145.0000000000000000 ) ) ;
#21074 = CARTESIAN_POINT ( 'NONE',  ( 158.0000000000007105, 138.2401247522676044, 45.00000000000000000 ) ) ;
#21075 = CARTESIAN_POINT ( 'NONE',  ( -273.6211430000234373, -91.18033988749901653, -14.64217782292691261 ) ) ;
#21076 = CIRCLE ( 'NONE', #8694, 19.07743405327024888 ) ;
#21077 = PLANE ( 'NONE',  #15603 ) ;
#21078 = AXIS2_PLACEMENT_3D ( 'NONE', #5877, #10479, #14939 ) ;
#21079 = CARTESIAN_POINT ( 'NONE',  ( -265.8568188415123359, -170.9585686148244292, -89.43929063625722620 ) ) ;
#21080 = CARTESIAN_POINT ( 'NONE',  ( -210.0000000000000853, -212.3568517473289603, 90.00000000000004263 ) ) ;
#21081 = CARTESIAN_POINT ( 'NONE',  ( -124.9781469243919076, 222.2250949724356985, -5.000000000000004441 ) ) ;
#21082 = CARTESIAN_POINT ( 'NONE',  ( 134.2103424514737640, 249.9921085342972162, -150.9609010065648249 ) ) ;
#21083 = CARTESIAN_POINT ( 'NONE',  ( -214.7594651349411379, 86.63962098186175353, 21.86053752875909240 ) ) ;
#21084 = LINE ( 'NONE', #24980, #9699 ) ;
#21085 = PLANE ( 'NONE',  #3573 ) ;
#21086 = DIRECTION ( 'NONE',  ( -0.000000000000000000, -0.000000000000000000, -1.000000000000000000 ) ) ;
#21087 = VERTEX_POINT ( 'NONE', #978 ) ;
#21088 = ADVANCED_FACE ( 'NONE', ( #11917 ), #23105, .T. ) ;
#21089 = CONICAL_SURFACE ( 'NONE', #3652, 5.999999999999977796, 1.029744258676652091 ) ;
#21090 = DIRECTION ( 'NONE',  ( -0.000000000000000000, -0.000000000000000000, 1.000000000000000000 ) ) ;
#21091 = CARTESIAN_POINT ( 'NONE',  ( 106.5442058163639985, 210.4990643932678438, -145.3948054049556902 ) ) ;
#21093 = EDGE_LOOP ( 'NONE', ( #10357, #13003, #10643, #8770 ) ) ;
#21092 = ORIENTED_EDGE ( 'NONE', *, *, #9177, .T. ) ;
#21094 = CIRCLE ( 'NONE', #3183, 30.00000000000000000 ) ;
#21095 = CARTESIAN_POINT ( 'NONE',  ( 158.0000000000010800, 103.1298746471690038, -45.00000000000000000 ) ) ;
#21096 = ORIENTED_EDGE ( 'NONE', *, *, #13847, .T. ) ;
#21097 = ORIENTED_EDGE ( 'NONE', *, *, #26038, .T. ) ;
#21098 = VERTEX_POINT ( 'NONE', #22685 ) ;
#21099 = EDGE_CURVE ( 'NONE', #14425, #7228, #14345, .T. ) ;
#21100 = EDGE_CURVE ( 'NONE', #15024, #15785, #10721, .T. ) ;
#21101 = EDGE_LOOP ( 'NONE', ( #13235, #12728, #22240, #6179 ) ) ;
#21102 = ORIENTED_EDGE ( 'NONE', *, *, #18092, .F. ) ;
#21103 = EDGE_LOOP ( 'NONE', ( #19979, #2176, #25659, #4522 ) ) ;
#21104 = DIRECTION ( 'NONE',  ( 0.000000000000000000, 0.000000000000000000, 1.000000000000000000 ) ) ;
#21105 = VECTOR ( 'NONE', #6096, 1000.000000000000000 ) ;
#21106 = CARTESIAN_POINT ( 'NONE',  ( 217.4999999999996305, 494.4107529906318632, -100.0000000000000142 ) ) ;
#21107 = CARTESIAN_POINT ( 'NONE',  ( -73.01279441628793165, 126.4618695315959087, 45.00000000000000000 ) ) ;
#21108 = ADVANCED_FACE ( 'NONE', ( #27257 ), #16185, .T. ) ;
#21109 = VECTOR ( 'NONE', #1709, 999.9999999999998863 ) ;
#21110 = CARTESIAN_POINT ( 'NONE',  ( -24.83510602130289513, 128.0375039002065023, -17.48817921712931067 ) ) ;
#21111 = EDGE_CURVE ( 'NONE', #24116, #22290, #3263, .T. ) ;
#21112 = CARTESIAN_POINT ( 'NONE',  ( -276.0340605539078638, -165.0395234928621448, -107.3883478461701912 ) ) ;
#21113 = PLANE ( 'NONE',  #22435 ) ;
#21114 = LINE ( 'NONE', #7904, #1950 ) ;
#21115 = DIRECTION ( 'NONE',  ( -0.000000000000000000, -0.000000000000000000, -1.000000000000000000 ) ) ;
#21116 = DIRECTION ( 'NONE',  ( 0.8379557447115549840, 0.5457381880580680633, 0.000000000000000000 ) ) ;
#21117 = CARTESIAN_POINT ( 'NONE',  ( 372.9108539694884144, 44.41075299063183479, 167.7200181511720416 ) ) ;
#21118 = PLANE ( 'NONE',  #4225 ) ;
#21119 = VERTEX_POINT ( 'NONE', #20939 ) ;
#21120 = DIRECTION ( 'NONE',  ( -0.6681556583950251094, -0.7440215159218921404, 0.000000000000000000 ) ) ;
#21121 = AXIS2_PLACEMENT_3D ( 'NONE', #12444, #18749, #1777 ) ;
#21122 = CARTESIAN_POINT ( 'NONE',  ( -279.1278187736259611, -165.0000000000001137, -106.1966075482098262 ) ) ;
#21123 = ORIENTED_EDGE ( 'NONE', *, *, #8742, .F. ) ;
#21124 = DIRECTION ( 'NONE',  ( -1.000000000000000000, 0.000000000000000000, 0.000000000000000000 ) ) ;
#21125 = ORIENTED_EDGE ( 'NONE', *, *, #23134, .F. ) ;
#21126 = ORIENTED_EDGE ( 'NONE', *, *, #15350, .T. ) ;
#21127 = EDGE_CURVE ( 'NONE', #3496, #8917, #11638, .T. ) ;
#21128 = AXIS2_PLACEMENT_3D ( 'NONE', #13621, #17630, #24524 ) ;
#21129 = EDGE_CURVE ( 'NONE', #21244, #1387, #24185, .T. ) ;
#21130 = CARTESIAN_POINT ( 'NONE',  ( 157.9999999999997158, 259.1260001201120531, 45.00000000000000000 ) ) ;
#21131 = DIRECTION ( 'NONE',  ( 0.000000000000000000, 0.000000000000000000, -1.000000000000000000 ) ) ;
#21132 = ORIENTED_EDGE ( 'NONE', *, *, #16504, .F. ) ;
#21133 = ORIENTED_EDGE ( 'NONE', *, *, #21742, .F. ) ;
#21134 = DIRECTION ( 'NONE',  ( 0.000000000000000000, 0.000000000000000000, -1.000000000000000000 ) ) ;
#21135 = DIRECTION ( 'NONE',  ( 0.000000000000000000, 0.000000000000000000, 1.000000000000000000 ) ) ;
#21136 = CARTESIAN_POINT ( 'NONE',  ( 157.9999999999997158, 259.1260001201120531, -45.00000000000000000 ) ) ;
#21137 = VERTEX_POINT ( 'NONE', #17568 ) ;
#21138 = CARTESIAN_POINT ( 'NONE',  ( 119.9999999999999147, 140.0000000000000000, 100.0000000000000142 ) ) ;
#21139 = ORIENTED_EDGE ( 'NONE', *, *, #17251, .F. ) ;
#21140 = CARTESIAN_POINT ( 'NONE',  ( -71.37541315349507443, 229.9999999999999716, 5.000000000000002665 ) ) ;
#21141 = EDGE_CURVE ( 'NONE', #28035, #16979, #4482, .T. ) ;
#21142 = VECTOR ( 'NONE', #21430, 1000.000000000000000 ) ;
#21143 = DIRECTION ( 'NONE',  ( 0.000000000000000000, 0.000000000000000000, 1.000000000000000000 ) ) ;
#21144 = DIRECTION ( 'NONE',  ( 0.3102637045530566295, -0.9506505318133544602, 0.000000000000000000 ) ) ;
#21145 = LINE ( 'NONE', #3334, #12232 ) ;
#21146 = DIRECTION ( 'NONE',  ( 0.000000000000000000, 0.000000000000000000, 1.000000000000000000 ) ) ;
#21147 = EDGE_CURVE ( 'NONE', #11070, #14636, #13001, .T. ) ;
#21148 = ADVANCED_FACE ( 'NONE', ( #26608 ), #20153, .F. ) ;
#21149 = VECTOR ( 'NONE', #9792, 1000.000000000000000 ) ;
#21150 = CARTESIAN_POINT ( 'NONE',  ( 163.3936278923558518, 210.3145496728149340, -146.5522648598509363 ) ) ;
#21151 = ORIENTED_EDGE ( 'NONE', *, *, #7748, .T. ) ;
#21152 = CARTESIAN_POINT ( 'NONE',  ( 217.4999999999996305, 258.6181251126050711, 1.387778780781445676E-14 ) ) ;
#21153 = ADVANCED_FACE ( 'NONE', ( #24467 ), #2188, .F. ) ;
#21154 = LINE ( 'NONE', #7287, #25719 ) ;
#21155 = FACE_OUTER_BOUND ( 'NONE', #22624, .T. ) ;
#21156 = PLANE ( 'NONE',  #8464 ) ;
#21157 = ORIENTED_EDGE ( 'NONE', *, *, #7641, .T. ) ;
#21158 = CARTESIAN_POINT ( 'NONE',  ( 5.999999999999999112, 5.000000000000000000, 0.000000000000000000 ) ) ;
#21159 = ORIENTED_EDGE ( 'NONE', *, *, #8054, .F. ) ;
#21160 = CARTESIAN_POINT ( 'NONE',  ( -186.1065741236299402, 106.0956363990103029, 31.60904046745896423 ) ) ;
#21161 = DIRECTION ( 'NONE',  ( 0.000000000000000000, 0.7071067811865476838, 0.7071067811865474617 ) ) ;
#21162 = CARTESIAN_POINT ( 'NONE',  ( 158.0000000000007958, 128.7164997297464595, -45.00000000000000000 ) ) ;
#21163 = VERTEX_POINT ( 'NONE', #19589 ) ;
#21164 = DIRECTION ( 'NONE',  ( 1.000000000000000000, 0.000000000000000000, 0.000000000000000000 ) ) ;
#21165 = CARTESIAN_POINT ( 'NONE',  ( 157.4999999999998579, 90.84443711338730054, 45.00000000000000000 ) ) ;
#21166 = VERTEX_POINT ( 'NONE', #10971 ) ;
#21167 = VECTOR ( 'NONE', #18060, 1000.000000000000000 ) ;
#21168 = LINE ( 'NONE', #10824, #19344 ) ;
#21169 = LINE ( 'NONE', #8243, #8539 ) ;
#21170 = ORIENTED_EDGE ( 'NONE', *, *, #6986, .T. ) ;
#21171 = VECTOR ( 'NONE', #364, 1000.000000000000000 ) ;
#21172 = ORIENTED_EDGE ( 'NONE', *, *, #4597, .F. ) ;
#21173 = DIRECTION ( 'NONE',  ( 0.000000000000000000, 0.000000000000000000, -1.000000000000000000 ) ) ;
#21174 = ORIENTED_EDGE ( 'NONE', *, *, #12847, .T. ) ;
#21175 = CIRCLE ( 'NONE', #27143, 6.000000000000005329 ) ;
#21176 = ORIENTED_EDGE ( 'NONE', *, *, #21439, .F. ) ;
#21177 = EDGE_LOOP ( 'NONE', ( #16510, #1385, #24928, #20558 ) ) ;
#21178 = LINE ( 'NONE', #25626, #153 ) ;
#21179 = DIRECTION ( 'NONE',  ( 0.000000000000000000, 0.000000000000000000, -1.000000000000000000 ) ) ;
#21180 = EDGE_CURVE ( 'NONE', #11217, #10760, #15717, .T. ) ;
#21181 = DIRECTION ( 'NONE',  ( 1.000000000000000000, 0.000000000000000000, 0.000000000000000000 ) ) ;
#21182 = EDGE_CURVE ( 'NONE', #27871, #1905, #9096, .T. ) ;
#21183 = CARTESIAN_POINT ( 'NONE',  ( 122.6339745962154808, 239.4185842870417389, 45.00000000000000000 ) ) ;
#21184 = DIRECTION ( 'NONE',  ( -1.000000000000000000, 0.000000000000000000, -0.000000000000000000 ) ) ;
#21185 = CARTESIAN_POINT ( 'NONE',  ( -222.4720504096164291, 61.14635810691093099, -21.27434031931761993 ) ) ;
#21186 = VECTOR ( 'NONE', #23918, 1000.000000000000000 ) ;
#21187 = ADVANCED_FACE ( 'NONE', ( #480 ), #21749, .F. ) ;
#21188 = CARTESIAN_POINT ( 'NONE',  ( 2.399999999999999911, 1.249999999999999556, -7.582700855991164168 ) ) ;
#21189 = DIRECTION ( 'NONE',  ( -0.8916010070296327417, 0.4528218681377311206, 0.000000000000000000 ) ) ;
#21191 = CARTESIAN_POINT ( 'NONE',  ( 158.0000000000013927, 75.54324956459154805, -45.00000000000000000 ) ) ;
#21190 = VECTOR ( 'NONE', #5054, 1000.000000000000000 ) ;
#21192 = LINE ( 'NONE', #28344, #8891 ) ;
#21193 = ORIENTED_EDGE ( 'NONE', *, *, #16901, .T. ) ;
#21194 = DIRECTION ( 'NONE',  ( 1.000000000000000000, 0.000000000000000000, 0.000000000000000000 ) ) ;
#21195 = PRESENTATION_LAYER_ASSIGNMENT (  '', '', ( #95 ) ) ;
#21196 = DIRECTION ( 'NONE',  ( -0.000000000000000000, -0.000000000000000000, 1.000000000000000000 ) ) ;
#21197 = FACE_OUTER_BOUND ( 'NONE', #3926, .T. ) ;
#21198 = CARTESIAN_POINT ( 'NONE',  ( -219.2467648448761395, 139.5102435001769265, -15.00000000000000000 ) ) ;
#21199 = DIRECTION ( 'NONE',  ( -0.8916010070295922185, -0.4528218681378110566, 0.000000000000000000 ) ) ;
#21200 = ORIENTED_EDGE ( 'NONE', *, *, #1452, .T. ) ;
#21201 = CARTESIAN_POINT ( 'NONE',  ( 232.4999999999996305, 194.4107529906318064, -75.35061095560291733 ) ) ;
#21202 = VERTEX_POINT ( 'NONE', #17427 ) ;
#21203 = DIRECTION ( 'NONE',  ( 1.321694076934710155E-16, -1.000000000000000000, 0.000000000000000000 ) ) ;
#21204 = VERTEX_POINT ( 'NONE', #6368 ) ;
#21205 = VECTOR ( 'NONE', #27029, 1000.000000000000227 ) ;
#21206 = VERTEX_POINT ( 'NONE', #10829 ) ;
#21207 = CARTESIAN_POINT ( 'NONE',  ( -47.90498801636491066, 130.8804178995914071, 16.39302846298827276 ) ) ;
#21208 = CIRCLE ( 'NONE', #12044, 1.000000000000000888 ) ;
#21209 = APPLICATION_CONTEXT ( 'automotive_design' ) ;
#21210 = ORIENTED_EDGE ( 'NONE', *, *, #8026, .T. ) ;
#21211 = VERTEX_POINT ( 'NONE', #6933 ) ;
#21212 = VECTOR ( 'NONE', #7703, 1000.000000000000114 ) ;
#21213 = CARTESIAN_POINT ( 'NONE',  ( 112.5876798426282619, 222.0498046809461812, 96.71269508460407849 ) ) ;
#21214 = LINE ( 'NONE', #14761, #10988 ) ;
#21215 = CARTESIAN_POINT ( 'NONE',  ( 158.0000000000007105, 136.2401247522676044, 45.00000000000000000 ) ) ;
#21216 = AXIS2_PLACEMENT_3D ( 'NONE', #21737, #11656, #11214 ) ;
#21217 = CARTESIAN_POINT ( 'NONE',  ( -144.7212326927123627, 126.7045300270324759, -16.81628189632150239 ) ) ;
#21218 = EDGE_CURVE ( 'NONE', #26389, #21355, #2330, .T. ) ;
#21219 = CARTESIAN_POINT ( 'NONE',  ( -268.0810832944869162, -170.6198684656366140, -94.21671656981227727 ) ) ;
#21220 = DIRECTION ( 'NONE',  ( 0.000000000000000000, 0.000000000000000000, -1.000000000000000000 ) ) ;
#21221 = CARTESIAN_POINT ( 'NONE',  ( 21.29940527161770092, -47.79570116690157988, 98.97008483812450663 ) ) ;
#21222 = CARTESIAN_POINT ( 'NONE',  ( -230.9605477664340185, 90.10120975743322447, -15.13325285068605730 ) ) ;
#21223 = ADVANCED_FACE ( 'NONE', ( #6512 ), #13895, .T. ) ;
#21224 = CARTESIAN_POINT ( 'NONE',  ( -175.0000000000000000, -170.0000000000001990, -64.00000000000000000 ) ) ;
#21225 = CARTESIAN_POINT ( 'NONE',  ( -226.9685481008362160, 87.85634458782620015, 15.93431596749161905 ) ) ;
#21226 = DIRECTION ( 'NONE',  ( -1.000000000000000000, 0.000000000000000000, 0.000000000000000000 ) ) ;
#21227 = CARTESIAN_POINT ( 'NONE',  ( 222.4999999999996021, 194.4107529906318064, 58.31593845887894645 ) ) ;
#21228 = DIRECTION ( 'NONE',  ( -0.8916010070297751833, -0.4528218681374507892, 0.000000000000000000 ) ) ;
#21229 = VERTEX_POINT ( 'NONE', #11404 ) ;
#21230 = VECTOR ( 'NONE', #15045, 1000.000000000000114 ) ;
#21231 = VECTOR ( 'NONE', #26416, 1000.000000000000000 ) ;
#21232 = CARTESIAN_POINT ( 'NONE',  ( -277.2150368962633706, -165.0000000000001421, -101.5769467933887995 ) ) ;
#21233 = CARTESIAN_POINT ( 'NONE',  ( 108.6319795274282143, 205.6865347771202721, -150.9608879355640170 ) ) ;
#21234 = AXIS2_PLACEMENT_3D ( 'NONE', #16334, #25083, #22929 ) ;
#21236 = EDGE_LOOP ( 'NONE', ( #9231, #120, #4268, #9310 ) ) ;
#21235 = EDGE_LOOP ( 'NONE', ( #23335, #24643 ) ) ;
#21237 = VECTOR ( 'NONE', #23646, 1000.000000000000000 ) ;
#21238 = CARTESIAN_POINT ( 'NONE',  ( 102.0697454929915295, 243.6045995028978837, -24.40655498894130915 ) ) ;
#21239 = VERTEX_POINT ( 'NONE', #20006 ) ;
#21240 = ORIENTED_EDGE ( 'NONE', *, *, #25718, .F. ) ;
#21241 = VERTEX_POINT ( 'NONE', #9241 ) ;
#21242 = ORIENTED_EDGE ( 'NONE', *, *, #24398, .F. ) ;
#21243 = EDGE_CURVE ( 'NONE', #11558, #21355, #15148, .T. ) ;
#21244 = VERTEX_POINT ( 'NONE', #26046 ) ;
#21245 = VERTEX_POINT ( 'NONE', #8953 ) ;
#21246 = LINE ( 'NONE', #3572, #27385 ) ;
#21247 = EDGE_CURVE ( 'NONE', #6227, #17385, #15293, .T. ) ;
#21248 = AXIS2_PLACEMENT_3D ( 'NONE', #14429, #5370, #3210 ) ;
#21249 = DIRECTION ( 'NONE',  ( 0.2588190451025321748, 0.9659258262890653146, 0.000000000000000000 ) ) ;
#21250 = TOROIDAL_SURFACE ( 'NONE', #12557, 60.59270260175150469, 2.000000000000000000 ) ;
#21251 = FACE_OUTER_BOUND ( 'NONE', #18807, .T. ) ;
#21252 = DIRECTION ( 'NONE',  ( -1.321694076934710155E-16, 1.000000000000000000, 0.000000000000000000 ) ) ;
#21253 = ADVANCED_FACE ( 'NONE', ( #13142 ), #5672, .T. ) ;
#21254 = CARTESIAN_POINT ( 'NONE',  ( 109.9999999999999432, -100.0000000000000142, 25.00000000000000711 ) ) ;
#21255 = FACE_BOUND ( 'NONE', #23010, .T. ) ;
#21256 = CARTESIAN_POINT ( 'NONE',  ( -214.5110300873075460, 71.95898175746583547, -27.23319810813256581 ) ) ;
#21257 = ADVANCED_FACE ( 'NONE', ( #48 ), #22166, .F. ) ;
#21258 = LINE ( 'NONE', #27567, #10944 ) ;
#21259 = FACE_OUTER_BOUND ( 'NONE', #2730, .T. ) ;
#21260 = CARTESIAN_POINT ( 'NONE',  ( 367.4999999999996021, -5.589247009368149222, 1.243177022048955014E-14 ) ) ;
#21261 = DIRECTION ( 'NONE',  ( 1.000000000000000000, 0.000000000000000000, 0.000000000000000000 ) ) ;
#21262 = ORIENTED_EDGE ( 'NONE', *, *, #27825, .T. ) ;
#21263 = CIRCLE ( 'NONE', #24470, 6.000000000000005329 ) ;
#21264 = CARTESIAN_POINT ( 'NONE',  ( -191.5097490750847555, 102.3060819963840231, 32.04619225362230139 ) ) ;
#21265 = VECTOR ( 'NONE', #18785, 1000.000000000000114 ) ;
#21266 = CARTESIAN_POINT ( 'NONE',  ( -276.0275629839314320, -165.0396948272157829, -107.3906533568332122 ) ) ;
#21267 = ORIENTED_EDGE ( 'NONE', *, *, #7378, .T. ) ;
#21268 = ITEM_DEFINED_TRANSFORMATION ( 'NONE', 'NONE', #6057,  #10637 ) ;
#21269 = AXIS2_PLACEMENT_3D ( 'NONE', #16201, #24949, #23076 ) ;
#21270 = VERTEX_POINT ( 'NONE', #22876 ) ;
#21271 = ADVANCED_FACE ( 'NONE', ( #4915, #26904 ), #7232, .T. ) ;
#21272 = ORIENTED_EDGE ( 'NONE', *, *, #22635, .F. ) ;
#21273 = CARTESIAN_POINT ( 'NONE',  ( 87.74278500254594348, 111.0010834410967959, 100.0000000000108429 ) ) ;
#21274 = CARTESIAN_POINT ( 'NONE',  ( 158.0000000000003126, 176.3661248723802828, -45.00000000000000000 ) ) ;
#21275 = ORIENTED_EDGE ( 'NONE', *, *, #25462, .F. ) ;
#21276 = VERTEX_POINT ( 'NONE', #20713 ) ;
#21277 = DIRECTION ( 'NONE',  ( -0.8916010070298462376, -0.4528218681373109011, 0.000000000000000000 ) ) ;
#21278 = EDGE_CURVE ( 'NONE', #8983, #21204, #9391, .T. ) ;
#21279 = CARTESIAN_POINT ( 'NONE',  ( 157.4999999999994600, 216.2381874887387880, -45.00000000000000000 ) ) ;
#21280 = CARTESIAN_POINT ( 'NONE',  ( -185.5167513424577237, 106.4752583619456914, -31.41993102962858231 ) ) ;
#21281 = ORIENTED_EDGE ( 'NONE', *, *, #24, .F. ) ;
#21282 = CARTESIAN_POINT ( 'NONE',  ( -231.9378824387731299, 93.53122965655670384, 13.00000000000000000 ) ) ;
#21283 = ORIENTED_EDGE ( 'NONE', *, *, #24019, .T. ) ;
#21284 = CIRCLE ( 'NONE', #6159, 7.108535549237485540 ) ;
#21285 = DIRECTION ( 'NONE',  ( -1.000000000000000000, 0.000000000000000000, 0.000000000000000000 ) ) ;
#21286 = LINE ( 'NONE', #14978, #1114 ) ;
#21287 = LINE ( 'NONE', #27742, #18168 ) ;
#21288 = VECTOR ( 'NONE', #26740, 1000.000000000000227 ) ;
#21289 = FACE_OUTER_BOUND ( 'NONE', #7558, .T. ) ;
#21290 = CARTESIAN_POINT ( 'NONE',  ( -229.2498027451138967, 132.0565166830976978, -13.00000000000000000 ) ) ;
#21291 = CARTESIAN_POINT ( 'NONE',  ( 163.2542326668747990, 209.9142827673095439, -147.6595947404202605 ) ) ;
#21292 = ORIENTED_EDGE ( 'NONE', *, *, #22126, .F. ) ;
#21293 = EDGE_CURVE ( 'NONE', #11731, #26795, #20438, .T. ) ;
#21294 = EDGE_CURVE ( 'NONE', #2548, #17145, #14265, .T. ) ;
#21295 = CARTESIAN_POINT ( 'NONE',  ( 217.4999999999996305, 258.6181251126050711, 1.387778780781445676E-14 ) ) ;
#21296 = DIRECTION ( 'NONE',  ( 1.000000000000000000, 0.000000000000000000, 0.000000000000000000 ) ) ;
#21297 = DIRECTION ( 'NONE',  ( -0.8916010070317489378, 0.4528218681335642870, 0.000000000000000000 ) ) ;
#21298 = LINE ( 'NONE', #6348, #10291 ) ;
#21299 = ORIENTED_EDGE ( 'NONE', *, *, #21986, .T. ) ;
#21300 = DIRECTION ( 'NONE',  ( 0.8916010070299578150, 0.4528218681370910770, 0.000000000000000000 ) ) ;
#21301 = DIRECTION ( 'NONE',  ( 0.000000000000000000, 0.000000000000000000, 1.000000000000000000 ) ) ;
#21302 = CARTESIAN_POINT ( 'NONE',  ( 158.0000000000013927, 75.54324956459154805, 45.00000000000000000 ) ) ;
#21303 = CARTESIAN_POINT ( 'NONE',  ( 157.4999999999998579, 93.35231212089433939, 45.00000000000000000 ) ) ;
#21304 = ORIENTED_EDGE ( 'NONE', *, *, #12436, .F. ) ;
#21305 = DIRECTION ( 'NONE',  ( 0.4528218681380902222, -0.8916010070294504430, 0.000000000000000000 ) ) ;
#21306 = CARTESIAN_POINT ( 'NONE',  ( 158.0000000000008527, 123.7007497147323960, -45.00000000000000000 ) ) ;
#21307 = ORIENTED_EDGE ( 'NONE', *, *, #664, .T. ) ;
#21308 = CIRCLE ( 'NONE', #9387, 30.00000000000001421 ) ;
#21309 = ADVANCED_FACE ( 'NONE', ( #13705 ), #22601, .F. ) ;
#21310 = DIRECTION ( 'NONE',  ( 0.000000000000000000, 1.000000000000000000, 0.000000000000000000 ) ) ;
#21311 = DIRECTION ( 'NONE',  ( 0.000000000000000000, -1.000000000000000000, 0.000000000000000000 ) ) ;
#21312 = VERTEX_POINT ( 'NONE', #5348 ) ;
#21313 = VECTOR ( 'NONE', #10891, 1000.000000000000000 ) ;
#21314 = ORIENTED_EDGE ( 'NONE', *, *, #7556, .F. ) ;
#21315 = EDGE_CURVE ( 'NONE', #3398, #24937, #1179, .T. ) ;
#21316 = CARTESIAN_POINT ( 'NONE',  ( 158.0000000000013927, 73.54324956459154805, 45.00000000000000000 ) ) ;
#21317 = ORIENTED_EDGE ( 'NONE', *, *, #26745, .F. ) ;
#21318 = EDGE_CURVE ( 'NONE', #10728, #16518, #18426, .T. ) ;
#21319 = VERTEX_POINT ( 'NONE', #11973 ) ;
#21320 = ORIENTED_EDGE ( 'NONE', *, *, #8426, .F. ) ;
#21321 = DIRECTION ( 'NONE',  ( -0.000000000000000000, -0.000000000000000000, -1.000000000000000000 ) ) ;
#21322 = DIRECTION ( 'NONE',  ( 0.4528218681371310450, -0.8916010070299376089, 0.000000000000000000 ) ) ;
#21323 = LINE ( 'NONE', #1119, #655 ) ;
#21324 = DIRECTION ( 'NONE',  ( 0.000000000000000000, 0.000000000000000000, 1.000000000000000000 ) ) ;
#21325 = AXIS2_PLACEMENT_3D ( 'NONE', #7460, #2993, #982 ) ;
#21326 = CARTESIAN_POINT ( 'NONE',  ( 114.7546517713170857, 220.0000000000000284, -189.9999999999999716 ) ) ;
#21327 = FACE_BOUND ( 'NONE', #20297, .T. ) ;
#21328 = CARTESIAN_POINT ( 'NONE',  ( -243.4193540313403901, 74.61988491600907025, -4.999999999761307379 ) ) ;
#21329 = VERTEX_POINT ( 'NONE', #27313 ) ;
#21330 = CARTESIAN_POINT ( 'NONE',  ( 157.9999999999996305, 288.7126252026890256, 45.00000000000000000 ) ) ;
#21331 = CIRCLE ( 'NONE', #12192, 6.000000000000005329 ) ;
#21332 = FACE_OUTER_BOUND ( 'NONE', #19543, .T. ) ;
#21333 = DIRECTION ( 'NONE',  ( 0.000000000000000000, 0.000000000000000000, 1.000000000000000000 ) ) ;
#21334 = LINE ( 'NONE', #1928, #3841 ) ;
#21335 = ORIENTED_EDGE ( 'NONE', *, *, #5735, .T. ) ;
#21336 = DIRECTION ( 'NONE',  ( 0.000000000000000000, 0.000000000000000000, -1.000000000000000000 ) ) ;
#21337 = CARTESIAN_POINT ( 'NONE',  ( 98.49253114489452798, 241.8754259314115416, -12.06625762472412333 ) ) ;
#21338 = CARTESIAN_POINT ( 'NONE',  ( -68.57415822541635464, 80.97823757117562593, 100.0000000000000000 ) ) ;
#21339 = SURFACE_SIDE_STYLE ('',( #5830 ) ) ;
#21340 = DIRECTION ( 'NONE',  ( 0.000000000000000000, 0.000000000000000000, -1.000000000000000000 ) ) ;
#21341 = ORIENTED_EDGE ( 'NONE', *, *, #7890, .F. ) ;
#21342 = CARTESIAN_POINT ( 'NONE',  ( 156.5461074670752453, 207.5603490538953224, -151.0000000000000284 ) ) ;
#21343 = VERTEX_POINT ( 'NONE', #11555 ) ;
#21344 = DIRECTION ( 'NONE',  ( -0.000000000000000000, -0.000000000000000000, -1.000000000000000000 ) ) ;
#21345 = ORIENTED_EDGE ( 'NONE', *, *, #21603, .T. ) ;
#21346 = AXIS2_PLACEMENT_3D ( 'NONE', #26912, #5354, #15871 ) ;
#21347 = EDGE_CURVE ( 'NONE', #8966, #16772, #16247, .T. ) ;
#21348 = AXIS2_PLACEMENT_3D ( 'NONE', #6840, #15622, #19635 ) ;
#21349 = VECTOR ( 'NONE', #12203, 1000.000000000000000 ) ;
#21350 = ORIENTED_EDGE ( 'NONE', *, *, #9014, .T. ) ;
#21351 = EDGE_CURVE ( 'NONE', #4661, #27627, #18150, .T. ) ;
#21352 = DIRECTION ( 'NONE',  ( -0.000000000000000000, -0.000000000000000000, -1.000000000000000000 ) ) ;
#21353 = ORIENTED_EDGE ( 'NONE', *, *, #18687, .T. ) ;
#21354 = VECTOR ( 'NONE', #14816, 1000.000000000000000 ) ;
#21355 = VERTEX_POINT ( 'NONE', #9808 ) ;
#21356 = CARTESIAN_POINT ( 'NONE',  ( 112.4997598733875606, 220.5042645990800168, 96.61410599988441561 ) ) ;
#21357 = CARTESIAN_POINT ( 'NONE',  ( -148.6329411077882980, 124.2076589707419316, -19.48823061374897847 ) ) ;
#21358 = CARTESIAN_POINT ( 'NONE',  ( 157.9999999999999716, 208.9684999699701393, 45.00000000000000000 ) ) ;
#21359 = CARTESIAN_POINT ( 'NONE',  ( -155.6066793474805934, 121.6020800752544773, -21.27933238366888347 ) ) ;
#21360 = DIRECTION ( 'NONE',  ( -0.8916010070296733758, -0.4528218681376511845, 0.000000000000000000 ) ) ;
#21361 = DIRECTION ( 'NONE',  ( -0.000000000000000000, 0.000000000000000000, -1.000000000000000000 ) ) ;
#21362 = CARTESIAN_POINT ( 'NONE',  ( -76.25760768171835480, 221.6666220619076739, -15.00000000000000000 ) ) ;
#21363 = CARTESIAN_POINT ( 'NONE',  ( -230.3334077407527900, 89.66896290591726881, -15.21539592855700107 ) ) ;
#21364 = CARTESIAN_POINT ( 'NONE',  ( 130.1183073479271002, 249.6003596541303011, -148.4939404368777218 ) ) ;
#21365 = VECTOR ( 'NONE', #14411, 1000.000000000000000 ) ;
#21366 = CARTESIAN_POINT ( 'NONE',  ( -220.0112564482956827, 86.21625987271094971, 18.70212642463580011 ) ) ;
#21367 = DIRECTION ( 'NONE',  ( 0.000000000000000000, -0.000000000000000000, -1.000000000000000000 ) ) ;
#21368 = DIRECTION ( 'NONE',  ( 0.8916010070293547418, 0.4528218681382786270, 0.000000000000000000 ) ) ;
#21369 = VECTOR ( 'NONE', #22792, 1000.000000000000000 ) ;
#21370 = DIRECTION ( 'NONE',  ( 0.000000000000000000, 0.000000000000000000, -1.000000000000000000 ) ) ;
#21371 = AXIS2_PLACEMENT_3D ( 'NONE', #7117, #20186, #4807 ) ;
#21372 = ORIENTED_EDGE ( 'NONE', *, *, #15203, .F. ) ;
#21373 = ADVANCED_FACE ( 'NONE', ( #5061 ), #19896, .T. ) ;
#21374 = DIRECTION ( 'NONE',  ( 0.4528218681383305855, -0.8916010070293283185, 0.000000000000000000 ) ) ;
#21375 = DIRECTION ( 'NONE',  ( 1.000000000000000000, 0.000000000000000000, -0.000000000000000000 ) ) ;
#21376 = CARTESIAN_POINT ( 'NONE',  ( 108.8204812537424715, 205.3442565862195863, -150.9999999999999716 ) ) ;
#21377 = AXIS2_PLACEMENT_3D ( 'NONE', #26408, #23986, #20235 ) ;
#21379 = EDGE_LOOP ( 'NONE', ( #5895, #23861 ) ) ;
#21378 = VERTEX_POINT ( 'NONE', #3325 ) ;
#21380 = CARTESIAN_POINT ( 'NONE',  ( 95.55652878160884711, 240.7834791927022593, -9.443977278911061646 ) ) ;
#21381 = ORIENTED_EDGE ( 'NONE', *, *, #13652, .F. ) ;
#21382 = ORIENTED_EDGE ( 'NONE', *, *, #4597, .T. ) ;
#21383 = ADVANCED_FACE ( 'NONE', ( #22742 ), #27041, .F. ) ;
#21384 = EDGE_LOOP ( 'NONE', ( #27613, #23792, #4418, #4792 ) ) ;
#21385 = EDGE_CURVE ( 'NONE', #1213, #5230, #11834, .T. ) ;
#21386 = EDGE_CURVE ( 'NONE', #2611, #3496, #16283, .T. ) ;
#21387 = EDGE_CURVE ( 'NONE', #27632, #17961, #15864, .T. ) ;
#21388 = EDGE_LOOP ( 'NONE', ( #6966, #11011, #8391, #6034 ) ) ;
#21389 = ORIENTED_EDGE ( 'NONE', *, *, #28250, .F. ) ;
#21390 = ORIENTED_EDGE ( 'NONE', *, *, #16682, .F. ) ;
#21391 = VECTOR ( 'NONE', #22059, 1000.000000000000000 ) ;
#21392 = CARTESIAN_POINT ( 'NONE',  ( 157.9999999999996305, 284.2047501951820436, 45.00000000000000000 ) ) ;
#21393 = CARTESIAN_POINT ( 'NONE',  ( -270.1025481742786951, -91.18033988749901653, -14.95564396479129243 ) ) ;
#21394 = VECTOR ( 'NONE', #19460, 1000.000000000000000 ) ;
#21395 = FACE_OUTER_BOUND ( 'NONE', #13952, .T. ) ;
#21396 = DIRECTION ( 'NONE',  ( 1.541976423090495387E-16, -1.000000000000000000, 0.000000000000000000 ) ) ;
#21397 = LINE ( 'NONE', #18962, #22714 ) ;
#21398 = DIRECTION ( 'NONE',  ( 0.000000000000000000, 0.000000000000000000, -1.000000000000000000 ) ) ;
#21399 = DIRECTION ( 'NONE',  ( 1.000000000000000000, 0.000000000000000000, 0.000000000000000000 ) ) ;
#21400 = CARTESIAN_POINT ( 'NONE',  ( -180.0000000000000284, -40.00000000000004974, 80.00000000000001421 ) ) ;
#21401 = CARTESIAN_POINT ( 'NONE',  ( -48.38593899427829115, 148.2549133597845241, 45.00000000000000000 ) ) ;
#21402 = DIRECTION ( 'NONE',  ( 0.000000000000000000, 0.000000000000000000, -1.000000000000000000 ) ) ;
#21403 = CARTESIAN_POINT ( 'NONE',  ( 157.4999999999998579, 151.0334372935563465, 45.00000000000000000 ) ) ;
#21404 = VERTEX_POINT ( 'NONE', #24611 ) ;
#21405 = AXIS2_PLACEMENT_3D ( 'NONE', #8534, #28189, #15433 ) ;
#21406 = CARTESIAN_POINT ( 'NONE',  ( -201.7499912683865091, 94.28702343169450728, 30.02677094166775973 ) ) ;
#21407 = ADVANCED_FACE ( 'NONE', ( #9670 ), #25036, .F. ) ;
#21408 = EDGE_CURVE ( 'NONE', #21673, #2119, #16698, .T. ) ;
#21409 = LINE ( 'NONE', #14531, #7153 ) ;
#21410 = ORIENTED_EDGE ( 'NONE', *, *, #20821, .T. ) ;
#21411 = ORIENTED_EDGE ( 'NONE', *, *, #14530, .F. ) ;
#21412 = VERTEX_POINT ( 'NONE', #21279 ) ;
#21413 = CARTESIAN_POINT ( 'NONE',  ( 91.70829090827390928, 81.72138244997330503, 100.0000000000000142 ) ) ;
#21414 = DIRECTION ( 'NONE',  ( 0.8916010070293710621, -0.4528218681382463195, 0.000000000000000000 ) ) ;
#21415 = ADVANCED_FACE ( 'NONE', ( #1734 ), #21680, .F. ) ;
#21416 = VERTEX_POINT ( 'NONE', #14682 ) ;
#21417 = ORIENTED_EDGE ( 'NONE', *, *, #17656, .T. ) ;
#21418 = CARTESIAN_POINT ( 'NONE',  ( 109.9999999999999147, 140.0000000000000000, -90.00000000000004263 ) ) ;
#21419 = EDGE_CURVE ( 'NONE', #25738, #9830, #5769, .T. ) ;
#21420 = FACE_OUTER_BOUND ( 'NONE', #14371, .T. ) ;
#21421 = CARTESIAN_POINT ( 'NONE',  ( -194.9019931824072671, 99.79035201896546425, -31.71427557561374400 ) ) ;
#21422 = ORIENTED_EDGE ( 'NONE', *, *, #12352, .T. ) ;
#21423 = FACE_OUTER_BOUND ( 'NONE', #20863, .T. ) ;
#21424 = ORIENTED_EDGE ( 'NONE', *, *, #22173, .T. ) ;
#21425 = VECTOR ( 'NONE', #21277, 1000.000000000000114 ) ;
#21426 = LINE ( 'NONE', #8504, #10241 ) ;
#21427 = CLOSED_SHELL ( 'NONE', ( #5199, #24984, #8422, #17360, #779, #16839, #25354, #21253, #16497, #11197, #23490, #24888, #26279 ) ) ;
#21428 = FACE_OUTER_BOUND ( 'NONE', #5784, .T. ) ;
#21429 = DIRECTION ( 'NONE',  ( 0.000000000000000000, -0.000000000000000000, -1.000000000000000000 ) ) ;
#21430 = DIRECTION ( 'NONE',  ( -0.000000000000000000, -0.000000000000000000, -1.000000000000000000 ) ) ;
#21431 = VERTEX_POINT ( 'NONE', #23298 ) ;
#21432 = CARTESIAN_POINT ( 'NONE',  ( -310.0000000000001137, -165.0000000000001137, 60.00000000000001421 ) ) ;
#21433 = CARTESIAN_POINT ( 'NONE',  ( 157.4999999999997158, 258.8720626163585621, -45.00000000000000000 ) ) ;
#21434 = DIRECTION ( 'NONE',  ( 0.000000000000000000, 0.000000000000000000, -1.000000000000000000 ) ) ;
#21435 = CARTESIAN_POINT ( 'NONE',  ( 267.4999999999996021, 194.4107529906318064, 288.0938197134494203 ) ) ;
#21436 = ORIENTED_EDGE ( 'NONE', *, *, #1339, .F. ) ;
#21437 = DIRECTION ( 'NONE',  ( -1.000000000000000000, 0.000000000000000000, 0.000000000000000000 ) ) ;
#21438 = EDGE_CURVE ( 'NONE', #19932, #21119, #3603, .T. ) ;
#21439 = EDGE_CURVE ( 'NONE', #2977, #12526, #18937, .T. ) ;
#21440 = DIRECTION ( 'NONE',  ( -0.000000000000000000, 0.000000000000000000, 1.000000000000000000 ) ) ;
#21441 = LINE ( 'NONE', #26031, #18381 ) ;
#21442 = CARTESIAN_POINT ( 'NONE',  ( -215.3193997209569091, 87.88581180658771075, 19.30547682902748718 ) ) ;
#21443 = EDGE_LOOP ( 'NONE', ( #23511, #10327, #5527, #14148 ) ) ;
#21444 = DIRECTION ( 'NONE',  ( 2.602085213965211135E-16, -1.000000000000000000, 0.000000000000000000 ) ) ;
#21445 = VERTEX_POINT ( 'NONE', #8070 ) ;
#21446 = AXIS2_PLACEMENT_3D ( 'NONE', #8606, #21529, #8467 ) ;
#21447 = DIRECTION ( 'NONE',  ( 0.8916010070295820045, 0.4528218681378310406, 0.000000000000000000 ) ) ;
#21448 = CARTESIAN_POINT ( 'NONE',  ( -194.9552809774316984, 99.75015356803743316, -32.14979201052287294 ) ) ;
#21449 = VERTEX_POINT ( 'NONE', #19124 ) ;
#21450 = EDGE_LOOP ( 'NONE', ( #23681, #17445, #3179 ) ) ;
#21451 = DIRECTION ( 'NONE',  ( 0.000000000000000000, -1.000000000000000000, 0.000000000000000000 ) ) ;
#21452 = EDGE_LOOP ( 'NONE', ( #22443, #10823, #13564, #9376 ) ) ;
#21453 = EDGE_CURVE ( 'NONE', #23180, #18280, #3893, .T. ) ;
#21454 = ADVANCED_FACE ( 'NONE', ( #16833 ), #27733, .F. ) ;
#21455 = ORIENTED_EDGE ( 'NONE', *, *, #4498, .F. ) ;
#21456 = EDGE_LOOP ( 'NONE', ( #4732, #17919, #22974, #9907, #1450 ) ) ;
#21457 = CARTESIAN_POINT ( 'NONE',  ( 179.9999999999999147, 526.4263741777961059, -100.0000000000000142 ) ) ;
#21458 = CIRCLE ( 'NONE', #25135, 30.00000000000000000 ) ;
#21459 = CIRCLE ( 'NONE', #17342, 5.000000000000004441 ) ;
#21460 = DIRECTION ( 'NONE',  ( 1.000000000000000000, -0.000000000000000000, -0.000000000000000000 ) ) ;
#21461 = CARTESIAN_POINT ( 'NONE',  ( 157.9999999999997442, 256.1102501050980322, -45.00000000000000000 ) ) ;
#21462 = DIRECTION ( 'NONE',  ( -0.000000000000000000, -0.000000000000000000, 1.000000000000000000 ) ) ;
#21463 = ADVANCED_FACE ( 'NONE', ( #21420 ), #8209, .F. ) ;
#21464 = DIRECTION ( 'NONE',  ( -0.000000000000000000, -0.000000000000000000, -1.000000000000000000 ) ) ;
#21465 = CARTESIAN_POINT ( 'NONE',  ( 119.9999999999999432, 2.220446049250311819E-14, -90.00000000000004263 ) ) ;
#21466 = CARTESIAN_POINT ( 'NONE',  ( -240.4233474261315564, 71.57180907112889656, -14.67903078147014462 ) ) ;
#21467 = ORIENTED_EDGE ( 'NONE', *, *, #17656, .F. ) ;
#21468 = EDGE_CURVE ( 'NONE', #5857, #11653, #2260, .T. ) ;
#21469 = DIRECTION ( 'NONE',  ( 1.000000000000000000, 0.000000000000000000, -0.000000000000000000 ) ) ;
#21470 = LINE ( 'NONE', #3519, #9718 ) ;
#21471 = DIRECTION ( 'NONE',  ( 1.000000000000000000, 2.602085213965211135E-16, -0.000000000000000000 ) ) ;
#21472 = LINE ( 'NONE', #16885, #12579 ) ;
#21473 = VERTEX_POINT ( 'NONE', #7013 ) ;
#21474 = CARTESIAN_POINT ( 'NONE',  ( -3.853576393533437815E-15, 1.249999999999999556, -7.097445415343742958 ) ) ;
#21475 = CIRCLE ( 'NONE', #11865, 5.000000000000004441 ) ;
#21476 = CARTESIAN_POINT ( 'NONE',  ( 157.4999999999996305, 288.9665627064425735, -45.00000000000000000 ) ) ;
#21477 = LINE ( 'NONE', #8696, #6863 ) ;
#21478 = CYLINDRICAL_SURFACE ( 'NONE', #23145, 5.999999999999977796 ) ;
#21479 = DIRECTION ( 'NONE',  ( 0.7071067811867438602, 0.000000000000000000, -0.7071067811863512853 ) ) ;
#21480 = CARTESIAN_POINT ( 'NONE',  ( 115.1711027725237528, 222.6105238444006886, -45.00000000000000000 ) ) ;
#21481 = EDGE_LOOP ( 'NONE', ( #1835, #17843, #25819, #11421 ) ) ;
#21482 = VECTOR ( 'NONE', #24372, 1000.000000000000000 ) ;
#21483 = CARTESIAN_POINT ( 'NONE',  ( 112.5248869502488986, 215.0130877889307044, -45.00000000000000000 ) ) ;
#21484 = ORIENTED_EDGE ( 'NONE', *, *, #14714, .T. ) ;
#21485 = DIRECTION ( 'NONE',  ( -0.000000000000000000, -0.000000000000000000, -1.000000000000000000 ) ) ;
#21486 = VECTOR ( 'NONE', #19068, 1000.000000000000000 ) ;
#21487 = ORIENTED_EDGE ( 'NONE', *, *, #4797, .F. ) ;
#21488 = ORIENTED_EDGE ( 'NONE', *, *, #21603, .F. ) ;
#21489 = CARTESIAN_POINT ( 'NONE',  ( 158.0000000000007390, 133.7322497447605656, 45.00000000000000000 ) ) ;
#21490 = EDGE_CURVE ( 'NONE', #17312, #23965, #26975, .T. ) ;
#21491 = ORIENTED_EDGE ( 'NONE', *, *, #5794, .F. ) ;
#21492 = ORIENTED_EDGE ( 'NONE', *, *, #14112, .F. ) ;
#21493 = PLANE ( 'NONE',  #10427 ) ;
#21494 = CARTESIAN_POINT ( 'NONE',  ( -100.1083977795999687, 134.3105318853753829, -15.54432045859607214 ) ) ;
#21495 = LINE ( 'NONE', #21358, #21230 ) ;
#21496 = AXIS2_PLACEMENT_3D ( 'NONE', #21542, #12661, #23848 ) ;
#21497 = CARTESIAN_POINT ( 'NONE',  ( -136.9828056817498805, 127.8991175801959486, -17.53799436710524873 ) ) ;
#21498 = CARTESIAN_POINT ( 'NONE',  ( -268.7670636128347041, -170.5295276737763857, -94.04889937631023145 ) ) ;
#21499 = VECTOR ( 'NONE', #10563, 1000.000000000000000 ) ;
#21500 = CARTESIAN_POINT ( 'NONE',  ( -266.6762645635436115, -170.8168138549905279, 94.53218878333569819 ) ) ;
#21501 = CARTESIAN_POINT ( 'NONE',  ( -223.1974999251100940, 88.61692301512375991, -14.90038877616663093 ) ) ;
#21502 = PRODUCT ( 'Rotating Grip', 'Rotating Grip', '', ( #21845 ) ) ;
#21503 = CARTESIAN_POINT ( 'NONE',  ( 129.6110901909775635, 249.5124271981383401, -142.3325995572698446 ) ) ;
#21504 = CARTESIAN_POINT ( 'NONE',  ( -261.1919288306253293, -171.9377729149742038, -94.99999999999987210 ) ) ;
#21505 = FACE_BOUND ( 'NONE', #4950, .T. ) ;
#21506 = CARTESIAN_POINT ( 'NONE',  ( 160.9807621135329612, 204.9999999999998863, -151.0000000000000284 ) ) ;
#21507 = CARTESIAN_POINT ( 'NONE',  ( 157.9999999999996305, 281.6968751876750616, 45.00000000000000000 ) ) ;
#21508 = EDGE_CURVE ( 'NONE', #19969, #8240, #4172, .T. ) ;
#21509 = ORIENTED_EDGE ( 'NONE', *, *, #24362, .T. ) ;
#21511 = EDGE_CURVE ( 'NONE', #18838, #2768, #4706, .T. ) ;
#21510 = VECTOR ( 'NONE', #27589, 1000.000000000000114 ) ;
#21512 = CIRCLE ( 'NONE', #6829, 24.07986109634097005 ) ;
#21513 = CARTESIAN_POINT ( 'NONE',  ( -2.862293735361731706E-14, 109.9999999999999858, 45.00000000000000000 ) ) ;
#21514 = DIRECTION ( 'NONE',  ( -1.000000000000000000, 6.752478448789676648E-18, 0.000000000000000000 ) ) ;
#21515 = EDGE_CURVE ( 'NONE', #13234, #1913, #11338, .T. ) ;
#21516 = CARTESIAN_POINT ( 'NONE',  ( -180.0000000000000284, -70.00000000000004263, 100.0000000000000142 ) ) ;
#21518 = VERTEX_POINT ( 'NONE', #7306 ) ;
#21517 = ORIENTED_EDGE ( 'NONE', *, *, #11410, .T. ) ;
#21519 = VECTOR ( 'NONE', #21582, 999.9999999999998863 ) ;
#21520 = CARTESIAN_POINT ( 'NONE',  ( 96.65725945967911059, 241.1367295422510040, -10.34535073431741026 ) ) ;
#21521 = EDGE_LOOP ( 'NONE', ( #20392, #18717, #25765, #10322 ) ) ;
#21522 = ORIENTED_EDGE ( 'NONE', *, *, #20699, .T. ) ;
#21523 = AXIS2_PLACEMENT_3D ( 'NONE', #5351, #22457, #13563 ) ;
#21524 = EDGE_LOOP ( 'NONE', ( #12297, #14050, #17560, #19722 ) ) ;
#21525 = AXIS2_PLACEMENT_3D ( 'NONE', #15238, #9046, #6458 ) ;
#21526 = EDGE_LOOP ( 'NONE', ( #17270, #15360, #25348, #21488 ) ) ;
#21527 = EDGE_LOOP ( 'NONE', ( #17126, #6854, #7365, #6192 ) ) ;
#21528 = VERTEX_POINT ( 'NONE', #17933 ) ;
#21529 = DIRECTION ( 'NONE',  ( -0.000000000000000000, 1.000000000000000000, -0.000000000000000000 ) ) ;
#21530 = AXIS2_PLACEMENT_3D ( 'NONE', #1572, #6166, #6021 ) ;
#21531 = DIRECTION ( 'NONE',  ( 0.8018642810807399268, 0.5975062131282553590, -0.000000000000000000 ) ) ;
#21532 = CARTESIAN_POINT ( 'NONE',  ( 105.9597133717324482, 242.8246303622935613, -29.94432334375205684 ) ) ;
#21533 = CARTESIAN_POINT ( 'NONE',  ( 157.4999999999998579, 186.1436873986549188, 45.00000000000000000 ) ) ;
#21534 = VECTOR ( 'NONE', #9933, 1000.000000000000000 ) ;
#21535=STYLED_ITEM('',(#28427),#27970);
#21536 = CARTESIAN_POINT ( 'NONE',  ( -263.2410596828399889, -166.3659179929189236, -109.9999999999998863 ) ) ;
#21537 = EDGE_CURVE ( 'NONE', #26048, #3858, #9307, .T. ) ;
#21538 = DIRECTION ( 'NONE',  ( -0.05364526231776645809, 0.9985600561963501320, 0.000000000000000000 ) ) ;
#21539 = CARTESIAN_POINT ( 'NONE',  ( -226.4322288603291611, 72.85292568147782788, -17.64883888685613655 ) ) ;
#21540 = ADVANCED_FACE ( 'NONE', ( #15798 ), #22533, .F. ) ;
#21541 = AXIS2_PLACEMENT_3D ( 'NONE', #8593, #11171, #28382 ) ;
#21542 = CARTESIAN_POINT ( 'NONE',  ( 157.4999999999998579, 178.6200623761337738, 45.00000000000000000 ) ) ;
#21543 = EDGE_CURVE ( 'NONE', #27217, #18668, #2697, .T. ) ;
#21544 = CARTESIAN_POINT ( 'NONE',  ( -310.0000000000001137, -165.0000000000000853, 60.00000000000002842 ) ) ;
#21545 = LINE ( 'NONE', #10492, #5552 ) ;
#21546 = DIRECTION ( 'NONE',  ( 0.8916010070298556744, -0.4528218681372921384, 0.000000000000000000 ) ) ;
#21547 = ORIENTED_EDGE ( 'NONE', *, *, #11378, .F. ) ;
#21548 = CARTESIAN_POINT ( 'NONE',  ( -177.6132461524688324, 111.0955659291485205, 29.96501893502363956 ) ) ;
#21549 = VECTOR ( 'NONE', #839, 1000.000000000000000 ) ;
#21550 = CARTESIAN_POINT ( 'NONE',  ( -274.6179956896274916, -170.0369464504329926, -102.6515880211471199 ) ) ;
#21551 = ORIENTED_EDGE ( 'NONE', *, *, #13619, .T. ) ;
#21552 = PRODUCT_CONTEXT ( 'NONE', #15356, 'mechanical' ) ;
#21553 = ORIENTED_EDGE ( 'NONE', *, *, #10019, .F. ) ;
#21554 = ORIENTED_EDGE ( 'NONE', *, *, #26457, .T. ) ;
#21555 = CARTESIAN_POINT ( 'NONE',  ( 82.68942924491597068, 110.0997128792283917, 100.0000000000000142 ) ) ;
#21556 = AXIS2_PLACEMENT_3D ( 'NONE', #22214, #11457, #15481 ) ;
#21557 = CARTESIAN_POINT ( 'NONE',  ( -175.0000000000000000, -120.0000000000001705, 76.00000000000001421 ) ) ;
#21558 = VERTEX_POINT ( 'NONE', #9174 ) ;
#21559 = ORIENTED_EDGE ( 'NONE', *, *, #25834, .F. ) ;
#21560 = CARTESIAN_POINT ( 'NONE',  ( 104.1118574119011555, 122.0584436052145918, -84.84374999967577935 ) ) ;
#21561 = VECTOR ( 'NONE', #27560, 1000.000000000000000 ) ;
#21562 = DIRECTION ( 'NONE',  ( 0.000000000000000000, 0.000000000000000000, -1.000000000000000000 ) ) ;
#21563 = CARTESIAN_POINT ( 'NONE',  ( 232.4999999999996305, 194.4107529906318348, 58.31593845887914540 ) ) ;
#21564 = VERTEX_POINT ( 'NONE', #28158 ) ;
#21565 = CARTESIAN_POINT ( 'NONE',  ( -220.2843281297837734, 86.23357641588329159, 18.56285956431874595 ) ) ;
#21566 = ORIENTED_EDGE ( 'NONE', *, *, #12906, .T. ) ;
#21567 = DIRECTION ( 'NONE',  ( 0.000000000000000000, 0.000000000000000000, -1.000000000000000000 ) ) ;
#21568 = EDGE_CURVE ( 'NONE', #26462, #5196, #2022, .T. ) ;
#21569 = EDGE_CURVE ( 'NONE', #3560, #10864, #2840, .T. ) ;
#21570 = DIRECTION ( 'NONE',  ( 0.4528218681371523058, 0.8916010070299268397, -0.000000000000000000 ) ) ;
#21571 = CARTESIAN_POINT ( 'NONE',  ( 157.4823930684554512, 200.1367640063166391, -144.2111520032349006 ) ) ;
#21572 = EDGE_CURVE ( 'NONE', #24562, #2081, #5141, .T. ) ;
#21573 = CARTESIAN_POINT ( 'NONE',  ( 0.000000000000000000, 0.000000000000000000, 45.00000000000000000 ) ) ;
#21574 = ORIENTED_EDGE ( 'NONE', *, *, #14419, .T. ) ;
#21575 = VECTOR ( 'NONE', #18478, 1000.000000000000114 ) ;
#21576 = CARTESIAN_POINT ( 'NONE',  ( -37.82257053376181233, 36.92584315232891612, 100.0000000000000000 ) ) ;
#21577 = ADVANCED_FACE ( 'NONE', ( #4991 ), #6870, .F. ) ;
#21578 = LINE ( 'NONE', #17267, #3697 ) ;
#21579 = CARTESIAN_POINT ( 'NONE',  ( 158.0000000000003126, 178.3661248723802828, 45.00000000000000000 ) ) ;
#21580 = CARTESIAN_POINT ( 'NONE',  ( 367.4999999999996021, 44.41075299063184900, 1.850330238640837654E-14 ) ) ;
#21581 = ORIENTED_EDGE ( 'NONE', *, *, #23785, .F. ) ;
#21582 = DIRECTION ( 'NONE',  ( 0.8916010070293584056, -0.4528218681382712996, 0.000000000000000000 ) ) ;
#21583 = AXIS2_PLACEMENT_3D ( 'NONE', #16714, #12414, #12273 ) ;
#21584 = PRODUCT_RELATED_PRODUCT_CATEGORY ( 'part', '', ( #21502 ) ) ;
#21585 = CARTESIAN_POINT ( 'NONE',  ( 65.00000000000000000, -170.0000000000000568, 70.00000000000001421 ) ) ;
#21586 = FACE_OUTER_BOUND ( 'NONE', #24810, .T. ) ;
#21587 = CARTESIAN_POINT ( 'NONE',  ( 134.9999999999998579, 220.0000000000000284, -45.00000000000000000 ) ) ;
#21588 = ORIENTED_EDGE ( 'NONE', *, *, #10014, .T. ) ;
#21589 = DIRECTION ( 'NONE',  ( -0.000000000000000000, -0.000000000000000000, 1.000000000000000000 ) ) ;
#21590 = EDGE_LOOP ( 'NONE', ( #26074, #3676, #11288, #20109 ) ) ;
#21591 = CARTESIAN_POINT ( 'NONE',  ( -144.0897808543928704, 125.7560339784919705, 18.58146195516149390 ) ) ;
#21592 = CARTESIAN_POINT ( 'NONE',  ( -169.2805883261569306, 115.5450669606412220, -26.60823203878023691 ) ) ;
#21593 = ORIENTED_EDGE ( 'NONE', *, *, #19238, .F. ) ;
#21594 = VERTEX_POINT ( 'NONE', #2551 ) ;
#21595 = DIRECTION ( 'NONE',  ( -0.8142945039115421224, -0.5804519453834706688, 0.000000000000000000 ) ) ;
#21596 = ORIENTED_EDGE ( 'NONE', *, *, #28077, .T. ) ;
#21597 = AXIS2_PLACEMENT_3D ( 'NONE', #12269, #25883, #8366 ) ;
#21599 = EDGE_CURVE ( 'NONE', #13260, #11332, #13493, .T. ) ;
#21598 = VERTEX_POINT ( 'NONE', #11634 ) ;
#21600 = ORIENTED_EDGE ( 'NONE', *, *, #10845, .F. ) ;
#21601 = CARTESIAN_POINT ( 'NONE',  ( 7.470826767499499255, 138.6324086774095576, 14.99999999999999822 ) ) ;
#21602 = VECTOR ( 'NONE', #6031, 1000.000000000000000 ) ;
#21603 = EDGE_CURVE ( 'NONE', #17930, #13771, #24543, .T. ) ;
#21604 = CYLINDRICAL_SURFACE ( 'NONE', #8059, 6.000000000000032863 ) ;
#21605 = CARTESIAN_POINT ( 'NONE',  ( -180.0000000000000284, -40.00000000000004974, -70.00000000000001421 ) ) ;
#21606 = LINE ( 'NONE', #10699, #1627 ) ;
#21607 = CARTESIAN_POINT ( 'NONE',  ( 107.9999999999998437, 220.0000000000000284, -119.9999999999999858 ) ) ;
#21608 = DIRECTION ( 'NONE',  ( 1.000000000000000000, 0.000000000000000000, 0.000000000000000000 ) ) ;
#21609 = CARTESIAN_POINT ( 'NONE',  ( -235.5733620266657340, 80.43390826602529842, -15.03591609561508946 ) ) ;
#21610 = ORIENTED_EDGE ( 'NONE', *, *, #16939, .T. ) ;
#21611 = DIRECTION ( 'NONE',  ( 2.602085213965211135E-16, -1.000000000000000000, 0.000000000000000000 ) ) ;
#21612 = EDGE_CURVE ( 'NONE', #23894, #16059, #16647, .T. ) ;
#21613 = DIRECTION ( 'NONE',  ( -0.000000000000000000, 0.000000000000000000, -1.000000000000000000 ) ) ;
#21614 = CARTESIAN_POINT ( 'NONE',  ( 123.9999999999998579, 220.0000000000000284, -99.00000000000001421 ) ) ;
#21615 = DIRECTION ( 'NONE',  ( 0.000000000000000000, -1.000000000000000000, 0.000000000000000000 ) ) ;
#21616 = EDGE_LOOP ( 'NONE', ( #22048, #453, #10953, #27630 ) ) ;
#21617 = DIRECTION ( 'NONE',  ( 1.000000000000000000, 0.000000000000000000, 0.000000000000000000 ) ) ;
#21618 = EDGE_CURVE ( 'NONE', #2305, #11934, #413, .T. ) ;
#21619 = AXIS2_PLACEMENT_3D ( 'NONE', #23212, #18895, #21189 ) ;
#21620 = DIRECTION ( 'NONE',  ( -0.8916010070296429557, -0.4528218681377111920, 0.000000000000000000 ) ) ;
#21621 = CARTESIAN_POINT ( 'NONE',  ( -274.7557459110829541, -165.0000000000001421, 86.12025961983462707 ) ) ;
#21622 = FACE_OUTER_BOUND ( 'NONE', #17518, .T. ) ;
#21623 = CARTESIAN_POINT ( 'NONE',  ( 157.9999999999996305, 286.7126252026890256, -45.00000000000000000 ) ) ;
#21624 = LINE ( 'NONE', #16892, #10639 ) ;
#21625 = VERTEX_POINT ( 'NONE', #7162 ) ;
#21626 = VECTOR ( 'NONE', #2356, 1000.000000000000000 ) ;
#21627 = VECTOR ( 'NONE', #25263, 1000.000000000000000 ) ;
#21628 = LINE ( 'NONE', #7996, #25829 ) ;
#21629 = ORIENTED_EDGE ( 'NONE', *, *, #14537, .T. ) ;
#21630 = DIRECTION ( 'NONE',  ( -0.000000000000000000, 1.000000000000000000, -1.387778780781445429E-16 ) ) ;
#21631 = VERTEX_POINT ( 'NONE', #15938 ) ;
#21632 = ADVANCED_FACE ( 'NONE', ( #27116 ), #12196, .F. ) ;
#21633 = ORIENTED_EDGE ( 'NONE', *, *, #1695, .F. ) ;
#21634 = LINE ( 'NONE', #11300, #3030 ) ;
#21635 = B_SPLINE_CURVE_WITH_KNOTS ( 'NONE', 3,
 ( #26974, #11770, #24829, #835, #27250, #25103, #7591, #5138, #1113, #13928, #22531, #3113, #16358, #20223, #9604, #18365, #555, #2695, #20652, #27384, #971, #24967, #5284, #14066, #24684, #18506, #15795, #5417 ),
 .UNSPECIFIED., .F., .F.,
 ( 4, 2, 2, 2, 2, 2, 2, 2, 2, 2, 2, 2, 2, 4 ),
 ( 3.469446951953614189E-18, 0.007613765012984346874, 0.01522753002596869028, 0.02284129503895303281, 0.02664817754544523271, 0.03045506005193743260, 0.04568259007790598236, 0.06091012010387453213, 0.07613765012984308189, 0.07994453263633524709, 0.08375141514282739841, 0.09136518015581171492, 0.1065927101817803480, 0.1218202402077489810 ),
 .UNSPECIFIED. ) ;
#21636 = EDGE_LOOP ( 'NONE', ( #11626, #7810, #5136, #2600 ) ) ;
#21637 = ORIENTED_EDGE ( 'NONE', *, *, #25821, .F. ) ;
#21638 = DIRECTION ( 'NONE',  ( 1.000000000000000000, 0.000000000000000000, -0.000000000000000000 ) ) ;
#21639 = DIRECTION ( 'NONE',  ( 0.000000000000000000, 0.000000000000000000, 1.000000000000000000 ) ) ;
#21640 = FACE_OUTER_BOUND ( 'NONE', #25260, .T. ) ;
#21641 = EDGE_CURVE ( 'NONE', #20791, #19423, #1255, .T. ) ;
#21642 = CIRCLE ( 'NONE', #25775, 5.999999999999991118 ) ;
#21643 = CARTESIAN_POINT ( 'NONE',  ( 134.9999999999998579, 220.0000000000000284, -99.00000000000001421 ) ) ;
#21644 = DIRECTION ( 'NONE',  ( 1.000000000000000000, 0.000000000000000000, -0.000000000000000000 ) ) ;
#21645 = VECTOR ( 'NONE', #27624, 1000.000000000000000 ) ;
#21646 = VECTOR ( 'NONE', #12741, 1000.000000000000000 ) ;
#21647 = CARTESIAN_POINT ( 'NONE',  ( -274.7130711414566235, -170.0340489564030690, -91.87824641412829862 ) ) ;
#21648 = CARTESIAN_POINT ( 'NONE',  ( -272.0864800775726167, -170.1925618487048268, 92.99347412766374532 ) ) ;
#21649 = CARTESIAN_POINT ( 'NONE',  ( -229.6379567168639539, 91.66739380564841611, -13.14213637420301062 ) ) ;
#21650 = CARTESIAN_POINT ( 'NONE',  ( 129.0001992662464829, 249.3939175884451629, -144.6008566625276615 ) ) ;
#21651 = FACE_OUTER_BOUND ( 'NONE', #12278, .T. ) ;
#21652 = FACE_OUTER_BOUND ( 'NONE', #21452, .T. ) ;
#21653 = DIRECTION ( 'NONE',  ( 0.000000000000000000, -1.000000000000000000, 0.000000000000000000 ) ) ;
#21654 = CARTESIAN_POINT ( 'NONE',  ( 157.4999999999998295, 40.68693696324645970, 45.00000000000000000 ) ) ;
#21655 = EDGE_LOOP ( 'NONE', ( #8105, #1272 ) ) ;
#21656 = ADVANCED_FACE ( 'NONE', ( #7450 ), #27253, .F. ) ;
#21657 = EDGE_CURVE ( 'NONE', #15640, #1333, #22955, .T. ) ;
#21658 = DIRECTION ( 'NONE',  ( -0.000000000000000000, 1.000000000000000000, -1.387778780781445429E-16 ) ) ;
#21659 = CARTESIAN_POINT ( 'NONE',  ( -0.000000000000000000, -280.0000000000000000, -110.0000000000000284 ) ) ;
#21660 = CARTESIAN_POINT ( 'NONE',  ( 108.1065091513366809, 206.7042902742356887, -150.6837522856750411 ) ) ;
#21661 = ORIENTED_EDGE ( 'NONE', *, *, #8352, .T. ) ;
#21662 = AXIS2_PLACEMENT_3D ( 'NONE', #8050, #5612, #5889 ) ;
#21663 = CARTESIAN_POINT ( 'NONE',  ( 107.1040180392036518, 249.6169203092518103, -26.84244457534687101 ) ) ;
#21664 = ORIENTED_EDGE ( 'NONE', *, *, #1773, .F. ) ;
#21665 = VERTEX_POINT ( 'NONE', #5710 ) ;
#21666 = AXIS2_PLACEMENT_3D ( 'NONE', #6045, #14825, #23576 ) ;
#21667 = ADVANCED_FACE ( 'NONE', ( #8009 ), #16775, .F. ) ;
#21668 = EDGE_LOOP ( 'NONE', ( #2289, #20078, #21844, #20433 ) ) ;
#21669 = AXIS2_PLACEMENT_3D ( 'NONE', #23119, #16795, #16242 ) ;
#21670 = ORIENTED_EDGE ( 'NONE', *, *, #23739, .T. ) ;
#21671 = VECTOR ( 'NONE', #18580, 1000.000000000000000 ) ;
#21672 = EDGE_LOOP ( 'NONE', ( #12078, #17179, #13519, #12981 ) ) ;
#21673 = VERTEX_POINT ( 'NONE', #10165 ) ;
#21674 = EDGE_CURVE ( 'NONE', #21229, #20572, #24431, .T. ) ;
#21675 = DIRECTION ( 'NONE',  ( -0.000000000000000000, 0.000000000000000000, -1.000000000000000000 ) ) ;
#21676 = EDGE_CURVE ( 'NONE', #2951, #21916, #19418, .T. ) ;
#21677 = FACE_OUTER_BOUND ( 'NONE', #4988, .T. ) ;
#21678 = EDGE_CURVE ( 'NONE', #23617, #11481, #1116, .T. ) ;
#21679 = CARTESIAN_POINT ( 'NONE',  ( -248.1546605714623013, -91.18033988749901653, 0.000000000000000000 ) ) ;
#21680 = CONICAL_SURFACE ( 'NONE', #25352, 6.025000000000002132, 0.7853981633971707232 ) ;
#21681 = LINE ( 'NONE', #12931, #24798 ) ;
#21682 = DIRECTION ( 'NONE',  ( 1.000000000000000000, 0.000000000000000000, 0.000000000000000000 ) ) ;
#21683 = CIRCLE ( 'NONE', #594, 44.99999999999998579 ) ;
#21684 = CARTESIAN_POINT ( 'NONE',  ( 217.4999999999996305, -5.589247009368136787, -100.0000000000000142 ) ) ;
#21685 = CIRCLE ( 'NONE', #9312, 43.76444293738737912 ) ;
#21686 = CARTESIAN_POINT ( 'NONE',  ( 156.9574749595459195, 226.9187638636467739, -45.00000000000000000 ) ) ;
#21687 = CARTESIAN_POINT ( 'NONE',  ( 158.0000000000002842, 178.8739998798873216, -45.00000000000000000 ) ) ;
#21688 = VECTOR ( 'NONE', #6683, 1000.000000000000000 ) ;
#21689 = DIRECTION ( 'NONE',  ( 1.000000000000000000, -0.000000000000000000, -0.000000000000000000 ) ) ;
#21690 = CARTESIAN_POINT ( 'NONE',  ( 65.00000000000000000, -120.0000000000000995, -69.99999999999998579 ) ) ;
#21691 = EDGE_CURVE ( 'NONE', #15333, #21229, #14483, .T. ) ;
#21692 = DIRECTION ( 'NONE',  ( -0.8916010070295820045, -0.4528218681378310406, 0.000000000000000000 ) ) ;
#21693 = CARTESIAN_POINT ( 'NONE',  ( 157.4999999999998579, 90.84443711338730054, 45.00000000000000000 ) ) ;
#21695 = EDGE_LOOP ( 'NONE', ( #26891, #11140, #13035, #23632 ) ) ;
#21694 = ORIENTED_EDGE ( 'NONE', *, *, #1662, .F. ) ;
#21696 = CARTESIAN_POINT ( 'NONE',  ( -181.2851160895673104, 108.9255553334400588, 31.23174333049976426 ) ) ;
#21697 = LINE ( 'NONE', #18973, #25946 ) ;
#21698 = ORIENTED_EDGE ( 'NONE', *, *, #13932, .T. ) ;
#21699 = APPLICATION_PROTOCOL_DEFINITION ( 'draft international standard', 'automotive_design', 1998, #10391 ) ;
#21700 = ORIENTED_EDGE ( 'NONE', *, *, #22342, .T. ) ;
#21701 = AXIS2_PLACEMENT_3D ( 'NONE', #17010, #23342, #10550 ) ;
#21702 = ORIENTED_EDGE ( 'NONE', *, *, #28314, .F. ) ;
#21703 = VECTOR ( 'NONE', #22045, 1000.000000000000114 ) ;
#21704 = PLANE ( 'NONE',  #19370 ) ;
#21705 = FACE_OUTER_BOUND ( 'NONE', #1945, .T. ) ;
#21706 = EDGE_LOOP ( 'NONE', ( #3850, #1102, #6952, #6370 ) ) ;
#21707 = AXIS2_PLACEMENT_3D ( 'NONE', #17203, #3979, #1966 ) ;
#21708 = ORIENTED_EDGE ( 'NONE', *, *, #17787, .T. ) ;
#21709 = EDGE_CURVE ( 'NONE', #26764, #11364, #11772, .T. ) ;
#21710 = CARTESIAN_POINT ( 'NONE',  ( 100.5794065449870942, 118.1137289701970872, -81.24999999966573228 ) ) ;
#21711 = EDGE_CURVE ( 'NONE', #13229, #23466, #23981, .T. ) ;
#21712 = CARTESIAN_POINT ( 'NONE',  ( 88.54392178150615678, 230.0000000000000284, 16.22216434841215360 ) ) ;
#21713 = CARTESIAN_POINT ( 'NONE',  ( -168.1663021066853787, 116.6858039761555119, -24.56336007714330449 ) ) ;
#21714 = ORIENTED_EDGE ( 'NONE', *, *, #19550, .F. ) ;
#21715 = CARTESIAN_POINT ( 'NONE',  ( -227.1642097121179233, 90.19069637679466211, 13.60986389833546717 ) ) ;
#21716 = ORIENTED_EDGE ( 'NONE', *, *, #13897, .F. ) ;
#21717 = DIRECTION ( 'NONE',  ( -0.000000000000000000, -0.000000000000000000, 1.000000000000000000 ) ) ;
#21718 = DIRECTION ( 'NONE',  ( -0.000000000000000000, 1.000000000000000000, -1.387778780781445429E-16 ) ) ;
#21719 = CARTESIAN_POINT ( 'NONE',  ( 157.6621827647630880, 200.3416932910694470, -143.0663072493378820 ) ) ;
#21720 = VECTOR ( 'NONE', #2029, 1000.000000000000000 ) ;
#21721 = PLANE ( 'NONE',  #47 ) ;
#21722 = ORIENTED_EDGE ( 'NONE', *, *, #24650, .F. ) ;
#21723 = AXIS2_PLACEMENT_3D ( 'NONE', #2473, #11261, #18289 ) ;
#21724 = CARTESIAN_POINT ( 'NONE',  ( 134.9999999999998579, 220.0000000000000284, -105.0000000000000284 ) ) ;
#21725 = EDGE_CURVE ( 'NONE', #10196, #14755, #5565, .T. ) ;
#21726 = CARTESIAN_POINT ( 'NONE',  ( -42.99650729631200363, 71.03850157808263077, 100.0000000000000000 ) ) ;
#21727 = CARTESIAN_POINT ( 'NONE',  ( 157.4999999999998579, 48.21056198576756202, 45.00000000000000000 ) ) ;
#21728 = VECTOR ( 'NONE', #13158, 999.9999999999998863 ) ;
#21729 = CARTESIAN_POINT ( 'NONE',  ( 158.0000000000001705, 190.9054999099155054, -45.00000000000000000 ) ) ;
#21730 = ORIENTED_EDGE ( 'NONE', *, *, #24150, .T. ) ;
#21731 = DIRECTION ( 'NONE',  ( -0.000000000000000000, -0.000000000000000000, -1.000000000000000000 ) ) ;
#21732 = ADVANCED_FACE ( 'NONE', ( #24970 ), #14342, .F. ) ;
#21733 = DIRECTION ( 'NONE',  ( -2.312964634635742464E-16, 1.000000000000000000, 0.000000000000000000 ) ) ;
#21734 = CARTESIAN_POINT ( 'NONE',  ( -17.24491960465746132, 75.97823757117562593, 80.00000000000001421 ) ) ;
#21735 = DIRECTION ( 'NONE',  ( -1.224646799147353207E-16, 0.000000000000000000, -1.000000000000000000 ) ) ;
#21736 = ORIENTED_EDGE ( 'NONE', *, *, #23009, .T. ) ;
#21737 = CARTESIAN_POINT ( 'NONE',  ( 157.9999999999999716, 210.9684999699701393, 45.00000000000000000 ) ) ;
#21738 = VERTEX_POINT ( 'NONE', #22817 ) ;
#21739 = LINE ( 'NONE', #28320, #27593 ) ;
#21740 = CARTESIAN_POINT ( 'NONE',  ( -160.8326600028555617, 120.2355194873574789, -21.37420696376538842 ) ) ;
#21741 = ORIENTED_EDGE ( 'NONE', *, *, #10039, .T. ) ;
#21742 = EDGE_CURVE ( 'NONE', #22223, #18214, #8843, .T. ) ;
#21743 = VECTOR ( 'NONE', #4635, 1000.000000000000000 ) ;
#21744 = VERTEX_POINT ( 'NONE', #18508 ) ;
#21745 = ADVANCED_FACE ( 'NONE', ( #5987 ), #26267, .T. ) ;
#21746 = CARTESIAN_POINT ( 'NONE',  ( 157.9999999999997726, 246.5866250825770294, -45.00000000000000000 ) ) ;
#21747 = ORIENTED_EDGE ( 'NONE', *, *, #26768, .F. ) ;
#21748 = PRODUCT_DEFINITION_SHAPE ( 'NONE', 'NONE',  #1224 ) ;
#21749 = PLANE ( 'NONE',  #7045 ) ;
#21750 = ADVANCED_FACE ( 'NONE', ( #3829 ), #10446, .F. ) ;
#21751 = EDGE_LOOP ( 'NONE', ( #16872, #5544, #20463, #17777 ) ) ;
#21752 = ORIENTED_EDGE ( 'NONE', *, *, #15722, .F. ) ;
#21753 = AXIS2_PLACEMENT_3D ( 'NONE', #14779, #24876, #18411 ) ;
#21754 = DIRECTION ( 'NONE',  ( -0.000000000000000000, 0.000000000000000000, -1.000000000000000000 ) ) ;
#21755 = DIRECTION ( 'NONE',  ( -0.000000000000000000, 1.000000000000000000, -1.387778780781445429E-16 ) ) ;
#21756 = CARTESIAN_POINT ( 'NONE',  ( 134.9999999999998579, 220.0000000000000284, -100.0000000000000142 ) ) ;
#21757 = CARTESIAN_POINT ( 'NONE',  ( 222.4999999999996021, 194.4107529906318064, -62.90796922943941638 ) ) ;
#21758 = CARTESIAN_POINT ( 'NONE',  ( -63.57415822541634043, 75.97823757117562593, 95.00000000000000000 ) ) ;
#21759 = CARTESIAN_POINT ( 'NONE',  ( 134.9999999999998579, 433.5940952139197293, -145.0000000000000000 ) ) ;
#21760 = CARTESIAN_POINT ( 'NONE',  ( -239.3181950532627980, 70.57797675263729786, -14.71337737011382352 ) ) ;
#21761 = VERTEX_POINT ( 'NONE', #6269 ) ;
#21762 = CARTESIAN_POINT ( 'NONE',  ( 157.9999999999997726, 243.5708750675630370, 45.00000000000000000 ) ) ;
#21763 = LINE ( 'NONE', #17872, #18452 ) ;
#21764 = FACE_OUTER_BOUND ( 'NONE', #13575, .T. ) ;
#21765 = DIRECTION ( 'NONE',  ( 0.000000000000000000, 0.000000000000000000, -1.000000000000000000 ) ) ;
#21766 = VERTEX_POINT ( 'NONE', #10305 ) ;
#21767 = AXIS2_PLACEMENT_3D ( 'NONE', #11530, #6631, #15407 ) ;
#21768 = CARTESIAN_POINT ( 'NONE',  ( 157.9999999999999147, 213.9842499849850697, -45.00000000000000000 ) ) ;
#21769 = CARTESIAN_POINT ( 'NONE',  ( -141.6428522700808230, 69.54464929955099706, 80.00000000000001421 ) ) ;
#21770 = CARTESIAN_POINT ( 'NONE',  ( 157.4999999999996305, 286.4586876989355915, 45.00000000000000000 ) ) ;
#21771 = PLANE ( 'NONE',  #22719 ) ;
#21772 = CARTESIAN_POINT ( 'NONE',  ( 294.9233831825460470, 127.6681916698403398, -138.9999999999999432 ) ) ;
#21773 = DIRECTION ( 'NONE',  ( -0.000000000000000000, 1.000000000000000000, -0.000000000000000000 ) ) ;
#21774 = AXIS2_PLACEMENT_3D ( 'NONE', #17484, #2250, #6284 ) ;
#21775 = ORIENTED_EDGE ( 'NONE', *, *, #9471, .F. ) ;
#21776 = ADVANCED_FACE ( 'NONE', ( #17326 ), #8437, .T. ) ;
#21777 = DIRECTION ( 'NONE',  ( 1.000000000000000000, 0.000000000000000000, 0.000000000000000000 ) ) ;
#21778 = ORIENTED_EDGE ( 'NONE', *, *, #5060, .T. ) ;
#21779 = DIRECTION ( 'NONE',  ( 0.000000000000000000, -0.000000000000000000, -1.000000000000000000 ) ) ;
#21780 = VERTEX_POINT ( 'NONE', #12896 ) ;
#21781 = VERTEX_POINT ( 'NONE', #12616 ) ;
#21782 = CARTESIAN_POINT ( 'NONE',  ( 157.4999999999998579, 176.1121873686267350, 45.00000000000000000 ) ) ;
#21783 = ADVANCED_FACE ( 'NONE', ( #21640 ), #8576, .F. ) ;
#21784 = EDGE_LOOP ( 'NONE', ( #20455, #12747 ) ) ;
#21785 = ORIENTED_EDGE ( 'NONE', *, *, #21025, .F. ) ;
#21786 = CARTESIAN_POINT ( 'NONE',  ( -219.9212092885508980, 137.1730549828704682, 15.11921763785538886 ) ) ;
#21787 = VECTOR ( 'NONE', #9042, 1000.000000000000227 ) ;
#21788 = DIRECTION ( 'NONE',  ( 1.000000000000000000, 0.000000000000000000, 0.000000000000000000 ) ) ;
#21789 = CARTESIAN_POINT ( 'NONE',  ( -213.0597602322721116, -217.1208202143830590, 94.62152100247507747 ) ) ;
#21790 = EDGE_CURVE ( 'NONE', #25403, #6335, #21495, .T. ) ;
#21791 = CARTESIAN_POINT ( 'NONE',  ( 158.0000000000008811, 123.1928747072253572, 45.00000000000000000 ) ) ;
#21792 = DIRECTION ( 'NONE',  ( 1.000000000000000000, -0.000000000000000000, -0.000000000000000000 ) ) ;
#21793 = VECTOR ( 'NONE', #20886, 1000.000000000000000 ) ;
#21794 = LINE ( 'NONE', #526, #5503 ) ;
#21795 = FACE_OUTER_BOUND ( 'NONE', #15776, .T. ) ;
#21796 = CARTESIAN_POINT ( 'NONE',  ( -227.1514737387478817, 90.13265483295766956, -13.57967572479353180 ) ) ;
#21797 = FACE_OUTER_BOUND ( 'NONE', #1451, .T. ) ;
#21798 = CARTESIAN_POINT ( 'NONE',  ( 113.4538925329242574, 207.5603490538955782, -138.9999999999999432 ) ) ;
#21799 = DIRECTION ( 'NONE',  ( 0.8660254037844432595, 0.4999999999999919509, 0.000000000000000000 ) ) ;
#21800 = DIRECTION ( 'NONE',  ( 1.000000000000000000, 0.000000000000000000, -0.000000000000000000 ) ) ;
#21801 = FACE_OUTER_BOUND ( 'NONE', #14190, .T. ) ;
#21802 = ORIENTED_EDGE ( 'NONE', *, *, #22266, .F. ) ;
#21803 = DIRECTION ( 'NONE',  ( -0.000000000000000000, -1.000000000000000000, -0.000000000000000000 ) ) ;
#21804 = LINE ( 'NONE', #1970, #5017 ) ;
#21805 = FACE_OUTER_BOUND ( 'NONE', #22774, .T. ) ;
#21806 = VECTOR ( 'NONE', #2097, 1000.000000000000000 ) ;
#21807 = CARTESIAN_POINT ( 'NONE',  ( 0.2651721261003159302, -1.250000000000000444, 7.393342869700422426 ) ) ;
#21808 = VERTEX_POINT ( 'NONE', #19064 ) ;
#21809 = VECTOR ( 'NONE', #11024, 1000.000000000000000 ) ;
#21810 = EDGE_CURVE ( 'NONE', #729, #26706, #23661, .T. ) ;
#21811 = CARTESIAN_POINT ( 'NONE',  ( 101.4665947576622216, 243.5985648160965980, -15.64809332290144006 ) ) ;
#21812 = ORIENTED_EDGE ( 'NONE', *, *, #20240, .T. ) ;
#21813 = EDGE_LOOP ( 'NONE', ( #19450, #15473 ) ) ;
#21814 = AXIS2_PLACEMENT_3D ( 'NONE', #9799, #12244, #18278 ) ;
#21815 = EDGE_LOOP ( 'NONE', ( #10759, #15505, #12965, #2980 ) ) ;
#21816 = ORIENTED_EDGE ( 'NONE', *, *, #7646, .T. ) ;
#21817 = ORIENTED_EDGE ( 'NONE', *, *, #18787, .F. ) ;
#21818 = ORIENTED_EDGE ( 'NONE', *, *, #25411, .F. ) ;
#21819 = DIRECTION ( 'NONE',  ( -0.000000000000000000, -0.000000000000000000, -1.000000000000000000 ) ) ;
#21820 = EDGE_CURVE ( 'NONE', #7097, #5376, #19201, .T. ) ;
#21821 = EDGE_CURVE ( 'NONE', #19430, #16733, #23373, .T. ) ;
#21822 = CARTESIAN_POINT ( 'NONE',  ( 367.4999999999996021, -5.589247009368160768, 100.0000000000000284 ) ) ;
#21823 = VECTOR ( 'NONE', #20585, 999.9999999999998863 ) ;
#21824 = CIRCLE ( 'NONE', #19526, 5.999999999999977796 ) ;
#21825 = VECTOR ( 'NONE', #9425, 1000.000000000000000 ) ;
#21826 = DIRECTION ( 'NONE',  ( -0.000000000000000000, -0.000000000000000000, -1.000000000000000000 ) ) ;
#21827 = CARTESIAN_POINT ( 'NONE',  ( -218.5620487852697522, 71.28382977987227775, 22.94473774458083071 ) ) ;
#21828 = LINE ( 'NONE', #19805, #20683 ) ;
#21829 = DIRECTION ( 'NONE',  ( 1.000000000000000000, 0.000000000000000000, 0.000000000000000000 ) ) ;
#21830 = CARTESIAN_POINT ( 'NONE',  ( 158.0000000000006537, 141.2558747672816821, -45.00000000000000000 ) ) ;
#21831 = CARTESIAN_POINT ( 'NONE',  ( 39.99999999999995026, -3.469446951953624838E-15, 100.0000000000000142 ) ) ;
#21832 = PLANE ( 'NONE',  #4471 ) ;
#21833 = CARTESIAN_POINT ( 'NONE',  ( 79.99999999999991473, 140.0000000000000000, -45.00000000000000000 ) ) ;
#21834 = ADVANCED_FACE ( 'NONE', ( #28233 ), #1812, .T. ) ;
#21835 = EDGE_CURVE ( 'NONE', #18558, #6129, #17191, .T. ) ;
#21836 = CARTESIAN_POINT ( 'NONE',  ( 109.7310248654090117, 203.8285304009907293, -150.8447356795924179 ) ) ;
#21837 = CARTESIAN_POINT ( 'NONE',  ( -175.8417606860892874, 246.9430296707336652, -13.00000000000000000 ) ) ;
#21838 = CARTESIAN_POINT ( 'NONE',  ( -277.2150368962633706, -237.2150368962634559, -104.9999999999998153 ) ) ;
#21839 = CARTESIAN_POINT ( 'NONE',  ( 158.0000000000005400, 153.7952498048169048, -45.00000000000000000 ) ) ;
#21841 = ORIENTED_EDGE ( 'NONE', *, *, #7733, .T. ) ;
#21840 = ORIENTED_EDGE ( 'NONE', *, *, #11907, .F. ) ;
#21842 = CARTESIAN_POINT ( 'NONE',  ( -162.7079589413399106, 119.3768178259787049, 22.14987655455460214 ) ) ;
#21843 = CARTESIAN_POINT ( 'NONE',  ( 157.4999999999998579, 133.4783122410070462, -45.00000000000000000 ) ) ;
#21844 = ORIENTED_EDGE ( 'NONE', *, *, #20672, .F. ) ;
#21845 = PRODUCT_CONTEXT ( 'NONE', #1202, 'mechanical' ) ;
#21846 = EDGE_CURVE ( 'NONE', #18918, #10018, #19368, .T. ) ;
#21847 = ORIENTED_EDGE ( 'NONE', *, *, #13363, .F. ) ;
#21848 = VECTOR ( 'NONE', #21414, 1000.000000000000114 ) ;
#21849 = ORIENTED_EDGE ( 'NONE', *, *, #2595, .T. ) ;
#21850 = FACE_OUTER_BOUND ( 'NONE', #5163, .T. ) ;
#21851 = LINE ( 'NONE', #23717, #18645 ) ;
#21852 = ORIENTED_EDGE ( 'NONE', *, *, #8387, .F. ) ;
#21853 =( BOUNDED_SURFACE ( )  B_SPLINE_SURFACE ( 3, 2, ( 
 ( #26888, #17693, #746 ),
 ( #22145, #22001, #15696 ),
 ( #7212, #322, #9076 ),
 ( #4464, #462, #13257 ),
 ( #7065, #11240, #26588 ),
 ( #24447, #2311, #24738 ),
 ( #22294, #15846, #11091 ),
 ( #26441, #22582, #24591 ),
 ( #24301, #4899, #13689 ),
 ( #20277, #9372, #3447 ) ),
 .UNSPECIFIED., .F., .F., .F. ) 
 B_SPLINE_SURFACE_WITH_KNOTS ( ( 4, 2, 2, 2, 4 ),
 ( 3, 3 ),
 ( 0.000000000000000000, 0.003993085574633944979, 0.007986171149267889957, 0.01197925672390183494, 0.01597234229853577991 ),
 ( 0.000000000000000000, 1.000000000000000000 ),
 .UNSPECIFIED. ) 
 GEOMETRIC_REPRESENTATION_ITEM ( )  RATIONAL_B_SPLINE_SURFACE ( (
 ( 1.000000000000000000, 0.7071067811865472397, 1.000000000000000000),
 ( 1.000000000000000000, 0.6986941146400569291, 1.000000000000000000),
 ( 1.000000000000000000, 0.6922065170621660712, 1.000000000000000000),
 ( 1.000000000000000000, 0.6834952607749176234, 1.000000000000000000),
 ( 1.000000000000000000, 0.6812778029564223736, 1.000000000000000000),
 ( 1.000000000000000000, 0.6812778029564223736, 1.000000000000000000),
 ( 1.000000000000000000, 0.6834952607775843791, 1.000000000000000000),
 ( 1.000000000000000000, 0.6922065170594993155, 1.000000000000000000),
 ( 1.000000000000000000, 0.6986941146420598825, 1.000000000000000000),
 ( 1.000000000000000000, 0.7071067811865472397, 1.000000000000000000) ) ) 
 REPRESENTATION_ITEM ( '' )  SURFACE ( )  );
#21854 = CIRCLE ( 'NONE', #8087, 1.999999999999996669 ) ;
#21855 = CARTESIAN_POINT ( 'NONE',  ( 107.3061218088456457, 127.3934823310315920, -100.0000000000216573 ) ) ;
#21856 = LINE ( 'NONE', #24579, #26100 ) ;
#21857 = VERTEX_POINT ( 'NONE', #26227 ) ;
#21858 = CARTESIAN_POINT ( 'NONE',  ( -214.2130517962793590, 88.01573912158703195, 20.10369910981496844 ) ) ;
#21859 = EDGE_LOOP ( 'NONE', ( #10690, #17810, #12578, #12276 ) ) ;
#21860 = CARTESIAN_POINT ( 'NONE',  ( -213.0248109774373972, -217.2055523511229467, 105.4731297167887902 ) ) ;
#21861 = LINE ( 'NONE', #24294, #18104 ) ;
#21862 = DIRECTION ( 'NONE',  ( -0.000000000000000000, 1.000000000000000000, -1.387778780781445429E-16 ) ) ;
#21863 = ORIENTED_EDGE ( 'NONE', *, *, #28127, .F. ) ;
#21864 = CARTESIAN_POINT ( 'NONE',  ( -140.1240808061633061, 61.15703788601673097, -683.1631314933625845 ) ) ;
#21865 = CARTESIAN_POINT ( 'NONE',  ( 167.4999999999996589, -5.589247009368136787, -74.99999999999995737 ) ) ;
#21866 = DIRECTION ( 'NONE',  ( 0.8660254037844394848, -0.4999999999999985012, 0.000000000000000000 ) ) ;
#21867 = CARTESIAN_POINT ( 'NONE',  ( -156.2917263574996127, 178.8555734514394828, 12.99999999999999822 ) ) ;
#21868 = ORIENTED_EDGE ( 'NONE', *, *, #7517, .T. ) ;
#21869 = FACE_BOUND ( 'NONE', #8271, .T. ) ;
#21870 = ADVANCED_FACE ( 'NONE', ( #14617 ), #16900, .T. ) ;
#21871 = LINE ( 'NONE', #15281, #24952 ) ;
#21872 = PLANE ( 'NONE',  #20412 ) ;
#21873 = ORIENTED_EDGE ( 'NONE', *, *, #21674, .F. ) ;
#21874 = EDGE_CURVE ( 'NONE', #465, #20505, #1363, .T. ) ;
#21875 = ORIENTED_EDGE ( 'NONE', *, *, #26982, .F. ) ;
#21876 = DIRECTION ( 'NONE',  ( -0.8916010070293584056, 0.4528218681382713551, 0.000000000000000000 ) ) ;
#21877 = CARTESIAN_POINT ( 'NONE',  ( -185.7285736283564006, 106.1028100233644125, -32.35901429591675083 ) ) ;
#21878 = ORIENTED_EDGE ( 'NONE', *, *, #22454, .F. ) ;
#21879 = AXIS2_PLACEMENT_3D ( 'NONE', #12397, #1453, #12536 ) ;
#21880 = VERTEX_POINT ( 'NONE', #24797 ) ;
#21881 = CARTESIAN_POINT ( 'NONE',  ( -111.1798965680916069, 69.38626228962301923, 82.93899756288178082 ) ) ;
#21882 = AXIS2_PLACEMENT_3D ( 'NONE', #21073, #27666, #14615 ) ;
#21883 = DIRECTION ( 'NONE',  ( 1.000000000000000000, 0.000000000000000000, 0.000000000000000000 ) ) ;
#21884 = ORIENTED_EDGE ( 'NONE', *, *, #24701, .T. ) ;
#21885 = ORIENTED_EDGE ( 'NONE', *, *, #23823, .F. ) ;
#21886 = CARTESIAN_POINT ( 'NONE',  ( -160.0000000000000284, 119.7660240611718763, 22.85081902853005431 ) ) ;
#21887 = EDGE_CURVE ( 'NONE', #9116, #11111, #16186, .T. ) ;
#21888 = LINE ( 'NONE', #17574, #20898 ) ;
#21889 = CARTESIAN_POINT ( 'NONE',  ( 158.0000000000011369, 98.11412463215494029, 45.00000000000000000 ) ) ;
#21890 = DIRECTION ( 'NONE',  ( -0.3102637045530777238, -0.9506505318133475768, 0.000000000000000000 ) ) ;
#21891 = DIRECTION ( 'NONE',  ( 0.8916010070298867607, 0.4528218681372308541, 0.000000000000000000 ) ) ;
#21892 = CARTESIAN_POINT ( 'NONE',  ( -209.8597496167328984, 64.07541194713586208, -30.05229862005789343 ) ) ;
#21893 = DIRECTION ( 'NONE',  ( 0.000000000000000000, -0.000000000000000000, 1.000000000000000000 ) ) ;
#21894 = ORIENTED_EDGE ( 'NONE', *, *, #24096, .F. ) ;
#21895 = CARTESIAN_POINT ( 'NONE',  ( 158.0000000000003126, 176.3661248723802828, 45.00000000000000000 ) ) ;
#21896 = ADVANCED_FACE ( 'NONE', ( #7273 ), #9989, .F. ) ;
#21897 = CARTESIAN_POINT ( 'NONE',  ( 157.9999999999997726, 244.0787500750700474, -45.00000000000000000 ) ) ;
#21898 = CARTESIAN_POINT ( 'NONE',  ( 157.9999999999996874, 264.1417501351260171, 45.00000000000000000 ) ) ;
#21899 = LINE ( 'NONE', #6673, #1990 ) ;
#21900 = VECTOR ( 'NONE', #24254, 1000.000000000000000 ) ;
#21901 = ORIENTED_EDGE ( 'NONE', *, *, #22423, .F. ) ;
#21902 = EDGE_CURVE ( 'NONE', #16933, #8650, #20902, .T. ) ;
#21903 = DIRECTION ( 'NONE',  ( 1.000000000000000000, 0.000000000000000000, -0.000000000000000000 ) ) ;
#21905 = EDGE_CURVE ( 'NONE', #18951, #27397, #19850, .T. ) ;
#21904 = CONICAL_SURFACE ( 'NONE', #9994, 6.025000000000002132, 0.7853981633974482790 ) ;
#21906 = ADVANCED_FACE ( 'NONE', ( #14038 ), #22785, .F. ) ;
#21907 = DIRECTION ( 'NONE',  ( 0.8916010070293783896, -0.4528218681382319422, 0.000000000000000000 ) ) ;
#21908 = LINE ( 'NONE', #17028, #27947 ) ;
#21909 = CARTESIAN_POINT ( 'NONE',  ( 130.0130877889309602, 242.4751130497508029, 45.00000000000000000 ) ) ;
#21910 = DIRECTION ( 'NONE',  ( 0.7071067811865474617, -0.7071067811865474617, 0.000000000000000000 ) ) ;
#21911 = CARTESIAN_POINT ( 'NONE',  ( 158.0000000000013927, 73.54324956459154805, -45.00000000000000000 ) ) ;
#21912 = ORIENTED_EDGE ( 'NONE', *, *, #5841, .T. ) ;
#21913 = CARTESIAN_POINT ( 'NONE',  ( -224.6762461164437354, 72.15359395014388610, 18.54889087295863348 ) ) ;
#21914 = ORIENTED_EDGE ( 'NONE', *, *, #10270, .T. ) ;
#21915 = FACE_OUTER_BOUND ( 'NONE', #27903, .T. ) ;
#21916 = VERTEX_POINT ( 'NONE', #5387 ) ;
#21917 = EDGE_LOOP ( 'NONE', ( #21126, #22315, #17743, #16355 ) ) ;
#21918 = LINE ( 'NONE', #26221, #2109 ) ;
#21919 = AXIS2_PLACEMENT_3D ( 'NONE', #11922, #22545, #9618 ) ;
#21920 = VERTEX_POINT ( 'NONE', #10132 ) ;
#21921 = ORIENTED_EDGE ( 'NONE', *, *, #27879, .F. ) ;
#21922 = CARTESIAN_POINT ( 'NONE',  ( -229.2498027451139251, 132.0565166830976693, 15.00000000000000000 ) ) ;
#21923 = CARTESIAN_POINT ( 'NONE',  ( 102.0697454929744907, 243.6045995028989068, 24.40655498896089171 ) ) ;
#21924 = DIRECTION ( 'NONE',  ( -1.000000000000000000, 0.000000000000000000, 0.000000000000000000 ) ) ;
#21925 = CARTESIAN_POINT ( 'NONE',  ( -40.40953891503691153, 0.000000000000000000, 99.00000000000000000 ) ) ;
#21926 = EDGE_CURVE ( 'NONE', #1420, #19053, #20757, .T. ) ;
#21927 = DIRECTION ( 'NONE',  ( 0.2588190451025121908, -0.9659258262890705327, 0.000000000000000000 ) ) ;
#21928 = ADVANCED_FACE ( 'NONE', ( #16460 ), #25210, .F. ) ;
#21929 = CARTESIAN_POINT ( 'NONE',  ( -210.0000000000000284, -3.238150488490040751E-14, -70.00000000000001421 ) ) ;
#21930 = FACE_OUTER_BOUND ( 'NONE', #1532, .T. ) ;
#21931 = CARTESIAN_POINT ( 'NONE',  ( 115.5814157129578916, 232.3660254037840502, 45.00000000000000000 ) ) ;
#21932 = LINE ( 'NONE', #20056, #20430 ) ;
#21933 = CARTESIAN_POINT ( 'NONE',  ( 157.4999999999994884, 211.2224374737238577, -45.00000000000000000 ) ) ;
#21934 = LINE ( 'NONE', #13191, #26517 ) ;
#21935 = CARTESIAN_POINT ( 'NONE',  ( 134.9999999999998863, 537.6859242279716682, 393.1631314933625845 ) ) ;
#21936 = EDGE_LOOP ( 'NONE', ( #659, #2506, #1140, #23968 ) ) ;
#21937 = DIRECTION ( 'NONE',  ( 0.000000000000000000, 0.000000000000000000, -1.000000000000000000 ) ) ;
#21938 = AXIS2_PLACEMENT_3D ( 'NONE', #4266, #10747, #23815 ) ;
#21939 = EDGE_CURVE ( 'NONE', #7303, #14397, #1223, .T. ) ;
#21940 = AXIS2_PLACEMENT_3D ( 'NONE', #26779, #24771, #7245 ) ;
#21941 = FACE_OUTER_BOUND ( 'NONE', #18119, .T. ) ;
#21942 = FACE_OUTER_BOUND ( 'NONE', #16962, .T. ) ;
#21943 = CARTESIAN_POINT ( 'NONE',  ( -8.294146619514105765E-15, -1.250000000000000222, 7.097209492490607730 ) ) ;
#21944 = ORIENTED_EDGE ( 'NONE', *, *, #19789, .T. ) ;
#21945 = CARTESIAN_POINT ( 'NONE',  ( 108.4669391322105412, 252.2354088788440549, -31.48703123558458472 ) ) ;
#21946 = ORIENTED_EDGE ( 'NONE', *, *, #15631, .F. ) ;
#21947 = DIRECTION ( 'NONE',  ( 0.8916010070293383105, -0.4528218681383106015, 0.000000000000000000 ) ) ;
#21948 = ORIENTED_EDGE ( 'NONE', *, *, #27441, .F. ) ;
#21949 = ORIENTED_EDGE ( 'NONE', *, *, #16816, .F. ) ;
#21950 = CIRCLE ( 'NONE', #4985, 10.00000000000000888 ) ;
#21951 = ORIENTED_EDGE ( 'NONE', *, *, #22716, .F. ) ;
#21952 = ORIENTED_EDGE ( 'NONE', *, *, #16016, .F. ) ;
#21953 = ORIENTED_EDGE ( 'NONE', *, *, #7790, .T. ) ;
#21954 = PLANE ( 'NONE',  #18245 ) ;
#21955 = VECTOR ( 'NONE', #22366, 1000.000000000000000 ) ;
#21956 = CIRCLE ( 'NONE', #19212, 30.00000000000000000 ) ;
#21957 = CARTESIAN_POINT ( 'NONE',  ( 158.0000000000006537, 143.2558747672816821, 45.00000000000000000 ) ) ;
#21958 = LINE ( 'NONE', #15083, #6134 ) ;
#21959 = CARTESIAN_POINT ( 'NONE',  ( -214.0383293111055139, 72.11341309493462859, 27.85175881924721608 ) ) ;
#21960 = DIRECTION ( 'NONE',  ( 1.000000000000000000, -0.000000000000000000, -0.000000000000000000 ) ) ;
#21961 = ADVANCED_FACE ( 'NONE', ( #3511 ), #12299, .F. ) ;
#21962 = CARTESIAN_POINT ( 'NONE',  ( 158.7404207507997853, 42.53436754635193040, 45.00000000000000000 ) ) ;
#21963 = CYLINDRICAL_SURFACE ( 'NONE', #11303, 9.999999999999991118 ) ;
#21964 = DIRECTION ( 'NONE',  ( -0.000000000000000000, -1.000000000000000000, -0.000000000000000000 ) ) ;
#21965 = DIRECTION ( 'NONE',  ( -0.000000000000000000, -0.000000000000000000, -1.000000000000000000 ) ) ;
#21966 = CARTESIAN_POINT ( 'NONE',  ( -232.6118856788241374, 77.06315004911816402, -15.48856666946770311 ) ) ;
#21968 = CARTESIAN_POINT ( 'NONE',  ( -33.73595832852618059, 129.3982092947608749, 15.58051948656918562 ) ) ;
#21967 = AXIS2_PLACEMENT_3D ( 'NONE', #22188, #4795, #13296 ) ;
#21969 = CARTESIAN_POINT ( 'NONE',  ( -140.1213116003368668, 122.5384136796733827, -15.00000000000000000 ) ) ;
#21970 = CARTESIAN_POINT ( 'NONE',  ( 372.9108539694884144, 44.41075299063183479, 100.0000000000000284 ) ) ;
#21971 = CARTESIAN_POINT ( 'NONE',  ( 157.4999999999996305, 288.9665627064425735, 45.00000000000000000 ) ) ;
#21973 = ORIENTED_EDGE ( 'NONE', *, *, #6073, .F. ) ;
#21972 = ORIENTED_EDGE ( 'NONE', *, *, #28050, .T. ) ;
#21974 = LINE ( 'NONE', #26287, #27941 ) ;
#21975 = VECTOR ( 'NONE', #24064, 1000.000000000000000 ) ;
#21976 = EDGE_CURVE ( 'NONE', #26678, #26198, #5811, .T. ) ;
#21977 = PRODUCT_DEFINITION_SHAPE ( 'NONE', 'NONE',  #186 ) ;
#21978 = EDGE_CURVE ( 'NONE', #15680, #9277, #14584, .T. ) ;
#21979 = CARTESIAN_POINT ( 'NONE',  ( -203.1779787704217313, 93.05164332230199875, -28.77272332722132830 ) ) ;
#21980 = EDGE_LOOP ( 'NONE', ( #18527, #8, #24356, #23996 ) ) ;
#21981 = ORIENTED_EDGE ( 'NONE', *, *, #23394, .F. ) ;
#21982 = ORIENTED_EDGE ( 'NONE', *, *, #14390, .F. ) ;
#21983 = CARTESIAN_POINT ( 'NONE',  ( 145.6339745962156940, 199.5814157129578064, 45.00000000000000000 ) ) ;
#21984 = CARTESIAN_POINT ( 'NONE',  ( -17.24491960465745777, -18.01420295945611727, 95.00000000000000000 ) ) ;
#21985 = ORIENTED_EDGE ( 'NONE', *, *, #7549, .F. ) ;
#21986 = EDGE_CURVE ( 'NONE', #18534, #4389, #3792, .T. ) ;
#21987 = CARTESIAN_POINT ( 'NONE',  ( 81.45493510946427307, 110.0000000030975400, -100.0000000000000142 ) ) ;
#21988 = EDGE_CURVE ( 'NONE', #21204, #2468, #21178, .T. ) ;
#21989 = AXIS2_PLACEMENT_3D ( 'NONE', #6697, #2098, #242 ) ;
#21990 = LINE ( 'NONE', #4455, #3616 ) ;
#21991 = CONICAL_SURFACE ( 'NONE', #431, 6.025000000000002132, 0.7853981633971707232 ) ;
#21992 = ORIENTED_EDGE ( 'NONE', *, *, #16273, .T. ) ;
#21993 = CARTESIAN_POINT ( 'NONE',  ( -227.1040115265393524, 87.91506694670529498, 15.89722369506078437 ) ) ;
#21994 = DIRECTION ( 'NONE',  ( 0.000000000000000000, -1.000000000000000000, 0.000000000000000000 ) ) ;
#21995 = VECTOR ( 'NONE', #22548, 1000.000000000000000 ) ;
#21996 = CARTESIAN_POINT ( 'NONE',  ( 150.5563491861040575, 203.0294372515228929, 45.00000000000000000 ) ) ;
#21997 = CARTESIAN_POINT ( 'NONE',  ( 157.5925105526923744, 200.2621716282842499, -146.5591841905931290 ) ) ;
#21998 = AXIS2_PLACEMENT_3D ( 'NONE', #18539, #18674, #14098 ) ;
#21999 = EDGE_LOOP ( 'NONE', ( #17288, #3884, #20826, #7476 ) ) ;
#22000 = FACE_OUTER_BOUND ( 'NONE', #11665, .T. ) ;
#22001 = CARTESIAN_POINT ( 'NONE',  ( -226.9034654752796314, 131.5715075451946348, -15.04814241297669319 ) ) ;
#22002 = DIRECTION ( 'NONE',  ( 0.4528218681381900867, -0.8916010070293997058, 0.000000000000000000 ) ) ;
#22003 = PLANE ( 'NONE',  #18550 ) ;
#22004 = ORIENTED_EDGE ( 'NONE', *, *, #15000, .F. ) ;
#22005 = DIRECTION ( 'NONE',  ( 1.000000000000000000, 0.000000000000000000, 0.000000000000000000 ) ) ;
#22006 = EDGE_CURVE ( 'NONE', #23905, #27805, #8114, .T. ) ;
#22007 = EDGE_CURVE ( 'NONE', #4103, #5352, #19164, .T. ) ;
#22008 = VECTOR ( 'NONE', #2666, 1000.000000000000000 ) ;
#22009 = LINE ( 'NONE', #9083, #5193 ) ;
#22010 = CARTESIAN_POINT ( 'NONE',  ( 216.4313787033304379, 124.9567147554451623, -45.00000000000000000 ) ) ;
#22011 = ORIENTED_EDGE ( 'NONE', *, *, #22490, .T. ) ;
#22012 =( NAMED_UNIT ( * ) SI_UNIT ( $, .STERADIAN. ) SOLID_ANGLE_UNIT ( ) );
#22013 = SHAPE_REPRESENTATION ( 'Drill Stand and Mount', ( #10637 ), #20272 ) ;
#22014 = ORIENTED_EDGE ( 'NONE', *, *, #13137, .T. ) ;
#22015 = AXIS2_PLACEMENT_3D ( 'NONE', #15890, #8978, #22335 ) ;
#22016 = DIRECTION ( 'NONE',  ( 1.000000000000000000, 0.000000000000000000, 0.000000000000000000 ) ) ;
#22017 = CARTESIAN_POINT ( 'NONE',  ( -185.2631373304065789, 106.4084716055997291, -32.26645048881131572 ) ) ;
#22018 = EDGE_LOOP ( 'NONE', ( #24963, #23000, #12492, #13666 ) ) ;
#22020 = EDGE_LOOP ( 'NONE', ( #20819, #13062, #17279, #20174 ) ) ;
#22019 = EDGE_CURVE ( 'NONE', #749, #20032, #10410, .T. ) ;
#22021 = CARTESIAN_POINT ( 'NONE',  ( 217.4999999999996305, 83.06687458711267880, -36.86484227207694175 ) ) ;
#22022 = DIRECTION ( 'NONE',  ( -0.8916010070294598799, 0.4528218681380715149, 0.000000000000000000 ) ) ;
#22023 = EDGE_LOOP ( 'NONE', ( #10580, #14613, #11797 ) ) ;
#22024 = ORIENTED_EDGE ( 'NONE', *, *, #6109, .T. ) ;
#22025 = EDGE_CURVE ( 'NONE', #6585, #23830, #17153, .T. ) ;
#22026 = CARTESIAN_POINT ( 'NONE',  ( 206.2214737538543829, 104.7347325308398354, -45.00000000000000000 ) ) ;
#22027 = EDGE_CURVE ( 'NONE', #3702, #9462, #22150, .T. ) ;
#22028 = AXIS2_PLACEMENT_3D ( 'NONE', #4822, #28370, #20200 ) ;
#22029 = CARTESIAN_POINT ( 'NONE',  ( 39.99999999999995026, -19.99999999999983302, 100.0000000000000142 ) ) ;
#22030 = ADVANCED_FACE ( 'NONE', ( #10274 ), #23085, .T. ) ;
#22031 = FACE_OUTER_BOUND ( 'NONE', #13659, .T. ) ;
#22032 = CARTESIAN_POINT ( 'NONE',  ( 8.415662294793918363, -4.274104551145060604, -45.00000000000000000 ) ) ;
#22033 = LINE ( 'NONE', #8962, #17817 ) ;
#22034 = CARTESIAN_POINT ( 'NONE',  ( -263.9162289044071485, -171.3140465951013311, 104.9290552840942325 ) ) ;
#22035 = CIRCLE ( 'NONE', #7812, 6.025000000000002132 ) ;
#22036 = PLANE ( 'NONE',  #8222 ) ;
#22037 = ORIENTED_EDGE ( 'NONE', *, *, #10845, .T. ) ;
#22038 = CARTESIAN_POINT ( 'NONE',  ( 128.0812361363527998, 241.9574749595457774, -45.00000000000000000 ) ) ;
#22039 = LINE ( 'NONE', #2345, #21186 ) ;
#22040 = DIRECTION ( 'NONE',  ( 0.000000000000000000, 0.000000000000000000, -1.000000000000000000 ) ) ;
#22041 = DIRECTION ( 'NONE',  ( 1.000000000000000000, 2.602085213965211135E-16, -0.000000000000000000 ) ) ;
#22042 = ORIENTED_EDGE ( 'NONE', *, *, #22889, .T. ) ;
#22043 = CARTESIAN_POINT ( 'NONE',  ( -212.8228108689316969, 60.01962377528477077, 15.18702394368705733 ) ) ;
#22044 = VERTEX_POINT ( 'NONE', #14874 ) ;
#22045 = DIRECTION ( 'NONE',  ( 0.8916010070295511403, -0.4528218681378915478, 0.000000000000000000 ) ) ;
#22046 = CARTESIAN_POINT ( 'NONE',  ( 158.0000000000010232, 106.1456246621830957, 45.00000000000000000 ) ) ;
#22047 = DIRECTION ( 'NONE',  ( 0.8153095126952236704, -0.5790253867566402812, 0.000000000000000000 ) ) ;
#22048 = ORIENTED_EDGE ( 'NONE', *, *, #1641, .F. ) ;
#22049 = CARTESIAN_POINT ( 'NONE',  ( 157.9999999999998010, 233.5393750375350237, 45.00000000000000000 ) ) ;
#22050 = SURFACE_STYLE_FILL_AREA ( #8837 ) ;
#22051 = ADVANCED_FACE ( 'NONE', ( #23620 ), #19308, .F. ) ;
#22052 = ORIENTED_EDGE ( 'NONE', *, *, #19623, .T. ) ;
#22053 = CIRCLE ( 'NONE', #6446, 429.0408555545579929 ) ;
#22054 = LINE ( 'NONE', #13305, #138 ) ;
#22055 = ORIENTED_EDGE ( 'NONE', *, *, #9290, .F. ) ;
#22056 = LINE ( 'NONE', #17602, #733 ) ;
#22057 = EDGE_LOOP ( 'NONE', ( #10636, #24748, #8572, #17002 ) ) ;
#22058 = VERTEX_POINT ( 'NONE', #27777 ) ;
#22059 = DIRECTION ( 'NONE',  ( -0.000000000000000000, -0.000000000000000000, -1.000000000000000000 ) ) ;
#22060 = VECTOR ( 'NONE', #21803, 1000.000000000000000 ) ;
#22061 = B_SPLINE_CURVE_WITH_KNOTS ( 'NONE', 3,
 ( #17973, #13115, #17539, #10804, #11231, #19560, #164, #24292, #13386, #13533, #28301, #21860, #10943, #2593, #19700, #312 ),
 .UNSPECIFIED., .F., .F.,
 ( 4, 2, 2, 2, 2, 2, 2, 4 ),
 ( 0.000000000000000000, 0.001557302553632665962, 0.002335953830448995582, 0.003114605107265324985, 0.004671907660898025859, 0.005450558937714371742, 0.005839884576122518663, 0.006229210214530665583 ),
 .UNSPECIFIED. ) ;
#22062 = ORIENTED_EDGE ( 'NONE', *, *, #25529, .T. ) ;
#22063 = ORIENTED_EDGE ( 'NONE', *, *, #15621, .T. ) ;
#22064 = CARTESIAN_POINT ( 'NONE',  ( -228.3260894844903532, 133.0445070941187851, 15.00000000000000000 ) ) ;
#22065 = EDGE_CURVE ( 'NONE', #17181, #27481, #28053, .T. ) ;
#22066 = CARTESIAN_POINT ( 'NONE',  ( 92.49170488790998945, 239.7529794472745834, 17.61766721976643879 ) ) ;
#22067 = ADVANCED_FACE ( 'NONE', ( #1914 ), #9778, .T. ) ;
#22068 = EDGE_CURVE ( 'NONE', #26043, #19122, #1500, .T. ) ;
#22069 = CARTESIAN_POINT ( 'NONE',  ( 232.4999999999996305, 83.06687458711267880, -30.86484227207694886 ) ) ;
#22070 = PLANE ( 'NONE',  #26595 ) ;
#22071 = CARTESIAN_POINT ( 'NONE',  ( 158.0000000000011937, 93.09837461714084839, 45.00000000000000000 ) ) ;
#22072 = CARTESIAN_POINT ( 'NONE',  ( -274.7557459110829541, -165.0000000000001137, 86.12025961983464128 ) ) ;
#22073 = CARTESIAN_POINT ( 'NONE',  ( 158.0000000000006537, 141.2558747672816821, 45.00000000000000000 ) ) ;
#22074 = AXIS2_PLACEMENT_3D ( 'NONE', #16370, #12204, #12061 ) ;
#22075 = CARTESIAN_POINT ( 'NONE',  ( 0.9552291512635501247, -1.249999999999998890, -7.454565938624087451 ) ) ;
#22076 = LINE ( 'NONE', #8862, #16767 ) ;
#22077 = CARTESIAN_POINT ( 'NONE',  ( -143.6428522700808230, 80.49308115506423178, 248.5795775865965993 ) ) ;
#22078 = CARTESIAN_POINT ( 'NONE',  ( 167.4999999999996589, 258.6181251126050711, 1.387778780781445676E-14 ) ) ;
#22079 = DIRECTION ( 'NONE',  ( -0.9506505318133506854, -0.3102637045530683979, 0.000000000000000000 ) ) ;
#22080 = EDGE_LOOP ( 'NONE', ( #20148, #20500, #3255, #22552 ) ) ;
#22081 = CARTESIAN_POINT ( 'NONE',  ( -24.92338318254763152, 127.6681916698425567, -137.0000000000000568 ) ) ;
#22082 = VECTOR ( 'NONE', #4867, 1000.000000000000000 ) ;
#22083 = DIRECTION ( 'NONE',  ( 1.000000000000000000, 0.000000000000000000, 0.000000000000000000 ) ) ;
#22084 = CARTESIAN_POINT ( 'NONE',  ( 157.4999999999998579, 143.5098122710352015, 45.00000000000000000 ) ) ;
#22085 = CARTESIAN_POINT ( 'NONE',  ( 107.5773805851584939, 207.8333816969443433, -139.9049692442121398 ) ) ;
#22086 = EDGE_LOOP ( 'NONE', ( #20115, #11877, #2882, #14336 ) ) ;
#22087 = CARTESIAN_POINT ( 'NONE',  ( 109.2338094452045425, 254.3984564254963630, -35.27666983503028320 ) ) ;
#22088 = ORIENTED_EDGE ( 'NONE', *, *, #3639, .T. ) ;
#22089 = DIRECTION ( 'NONE',  ( 0.4528218681373308296, -0.8916010070298360235, 0.000000000000000000 ) ) ;
#22090 = ORIENTED_EDGE ( 'NONE', *, *, #21790, .F. ) ;
#22091 = VERTEX_POINT ( 'NONE', #16874 ) ;
#22092 = AXIS2_PLACEMENT_3D ( 'NONE', #17336, #5997, #1823 ) ;
#22093 = ORIENTED_EDGE ( 'NONE', *, *, #6027, .T. ) ;
#22094 = ORIENTED_EDGE ( 'NONE', *, *, #7486, .F. ) ;
#22095 = VECTOR ( 'NONE', #6222, 999.9999999999998863 ) ;
#22096 = ORIENTED_EDGE ( 'NONE', *, *, #18841, .F. ) ;
#22097 = AXIS2_PLACEMENT_3D ( 'NONE', #20324, #15746, #4802 ) ;
#22098 = CARTESIAN_POINT ( 'NONE',  ( 367.9108539694884144, -5.589247009368160768, 100.0000000000000284 ) ) ;
#22099 = ADVANCED_FACE ( 'NONE', ( #23479 ), #12719, .F. ) ;
#22100 = CIRCLE ( 'NONE', #4185, 21.59849023212046149 ) ;
#22101 = B_SPLINE_CURVE_WITH_KNOTS ( 'NONE', 3,
 ( #9423, #24787, #22775, #5094, #25068, #11864, #5379, #14158, #22910, #3217, #12003, #11589, #20327, #1071, #9839, #18597, #27345, #25200, #14297, #23051, #3359, #8388, #21591, #25612, #25899, #28184, #27764, #10261 ),
 .UNSPECIFIED., .F., .F.,
 ( 4, 2, 2, 2, 2, 2, 2, 2, 2, 2, 2, 2, 2, 4 ),
 ( 0.000000000000000000, 0.01499785927852794604, 0.02999571855705591289, 0.03749464819631988938, 0.04124411301595189844, 0.04499357783558391444, 0.05999143711411201313, 0.07498929639264009794, 0.08998715567116818970, 0.09373662049080021264, 0.09748608531043220782, 0.1049850149496963231, 0.1124839445889604245, 0.1199828742282245259 ),
 .UNSPECIFIED. ) ;
#22102 = EDGE_CURVE ( 'NONE', #26043, #17587, #19452, .T. ) ;
#22103 = CARTESIAN_POINT ( 'NONE',  ( 232.4749999999995964, 133.0668745871126930, 36.86484227207694886 ) ) ;
#22104 = CARTESIAN_POINT ( 'NONE',  ( 137.6105238444012286, 200.1711027725236534, 45.00000000000000000 ) ) ;
#22105 = CARTESIAN_POINT ( 'NONE',  ( -199.5809478526699650, 61.42778479158862126, 28.44561038856815927 ) ) ;
#22106 = FACE_OUTER_BOUND ( 'NONE', #13098, .T. ) ;
#22107 = DIRECTION ( 'NONE',  ( -0.8916010070299166257, 0.4528218681371722343, 0.000000000000000000 ) ) ;
#22108 = FACE_OUTER_BOUND ( 'NONE', #9707, .T. ) ;
#22109 = DIRECTION ( 'NONE',  ( 1.000000000000000000, 0.000000000000000000, 0.000000000000000000 ) ) ;
#22110 = DIRECTION ( 'NONE',  ( -0.000000000000000000, -0.000000000000000000, -1.000000000000000000 ) ) ;
#22111 = FACE_BOUND ( 'NONE', #24993, .T. ) ;
#22112 = VECTOR ( 'NONE', #27468, 1000.000000000000000 ) ;
#22113 = CARTESIAN_POINT ( 'NONE',  ( 0.6954374052207565882, 136.6090791541018632, 13.39223910979635690 ) ) ;
#22114 = CARTESIAN_POINT ( 'NONE',  ( -138.6428522700808230, 66.54464929955099706, 83.00000000000001421 ) ) ;
#22115 = CARTESIAN_POINT ( 'NONE',  ( 372.9108539694884144, 44.41075299063183479, 100.0000000000000284 ) ) ;
#22116 = CARTESIAN_POINT ( 'NONE',  ( -200.0000000000000284, -91.18033988749901653, -21.20097097723064294 ) ) ;
#22117 = VECTOR ( 'NONE', #25159, 1000.000000000000000 ) ;
#22119 = ORIENTED_EDGE ( 'NONE', *, *, #19988, .F. ) ;
#22118 = ORIENTED_EDGE ( 'NONE', *, *, #1605, .F. ) ;
#22120 = PRODUCT_DEFINITION_FORMATION_WITH_SPECIFIED_SOURCE ( 'ANY', '', #6610, .NOT_KNOWN. ) ;
#22121 = CARTESIAN_POINT ( 'NONE',  ( -160.8326600028555902, 120.2355194873574931, 21.37420696376537776 ) ) ;
#22122 = CARTESIAN_POINT ( 'NONE',  ( -205.8155715011940288, 91.09379270857378685, -26.99297343021914131 ) ) ;
#22123 = EDGE_LOOP ( 'NONE', ( #868, #15685, #13893 ) ) ;
#22124 = ORIENTED_EDGE ( 'NONE', *, *, #1961, .T. ) ;
#22125 = ORIENTED_EDGE ( 'NONE', *, *, #16841, .F. ) ;
#22126 = EDGE_CURVE ( 'NONE', #16598, #18699, #3230, .T. ) ;
#22127 = CARTESIAN_POINT ( 'NONE',  ( -40.40953891503691153, 0.000000000000000000, 100.0000000000000000 ) ) ;
#22128 = CARTESIAN_POINT ( 'NONE',  ( -127.7167972290761071, 131.6999243923856397, 16.10307571226574197 ) ) ;
#22129 = ORIENTED_EDGE ( 'NONE', *, *, #26195, .T. ) ;
#22130 = VECTOR ( 'NONE', #18609, 1000.000000000000227 ) ;
#22131 = CYLINDRICAL_SURFACE ( 'NONE', #9976, 29.99999999999999645 ) ;
#22132 = AXIS2_PLACEMENT_3D ( 'NONE', #4305, #2144, #6739 ) ;
#22133 = EDGE_CURVE ( 'NONE', #28048, #17557, #51, .T. ) ;
#22134 = CARTESIAN_POINT ( 'NONE',  ( 158.0000000000009095, 120.6849996997183183, -45.00000000000000000 ) ) ;
#22135 = ORIENTED_EDGE ( 'NONE', *, *, #8809, .T. ) ;
#22136 = CARTESIAN_POINT ( 'NONE',  ( -207.8784783882069860, 89.22626204389251825, 26.87087741168311084 ) ) ;
#22137 = TOROIDAL_SURFACE ( 'NONE', #15712, 33.76444293738737912, 9.999999999999996447 ) ;
#22138 = DIRECTION ( 'NONE',  ( -0.000000000000000000, 0.000000000000000000, -1.000000000000000000 ) ) ;
#22139 = CIRCLE ( 'NONE', #16192, 32.49120955644046660 ) ;
#22140 = EDGE_CURVE ( 'NONE', #1515, #9431, #11409, .T. ) ;
#22141 = DIRECTION ( 'NONE',  ( -0.000000000000000000, 1.000000000000000000, -0.000000000000000000 ) ) ;
#22142 = CARTESIAN_POINT ( 'NONE',  ( 157.4559486869681848, 200.1070271554761462, -145.3948054049556902 ) ) ;
#22143 = VERTEX_POINT ( 'NONE', #17715 ) ;
#22144 = DIRECTION ( 'NONE',  ( 1.000000000000000000, 0.000000000000000000, 0.000000000000000000 ) ) ;
#22145 = CARTESIAN_POINT ( 'NONE',  ( -228.3260894844903817, 133.0445070941187851, -15.00000000000000178 ) ) ;
#22146 = CARTESIAN_POINT ( 'NONE',  ( -210.0000000000000284, -157.0000000000000284, -105.0000000000000284 ) ) ;
#22147 = FACE_OUTER_BOUND ( 'NONE', #21527, .T. ) ;
#22148 = EDGE_LOOP ( 'NONE', ( #8392, #27773, #17043, #3188 ) ) ;
#22149 = EDGE_CURVE ( 'NONE', #23617, #10961, #26742, .T. ) ;
#22150 = CIRCLE ( 'NONE', #21701, 72.21503689626329958 ) ;
#22151 = DIRECTION ( 'NONE',  ( -0.000000000000000000, -0.000000000000000000, -1.000000000000000000 ) ) ;
#22152 = AXIS2_PLACEMENT_3D ( 'NONE', #23924, #5583, #19609 ) ;
#22153 = CARTESIAN_POINT ( 'NONE',  ( 81.39309752945497678, 249.3891174404998594, 45.00000000000000000 ) ) ;
#22154 = LINE ( 'NONE', #4616, #23163 ) ;
#22155 = EDGE_LOOP ( 'NONE', ( #1863, #26804, #15500, #13891 ) ) ;
#22156 =( LENGTH_UNIT ( ) NAMED_UNIT ( * ) SI_UNIT ( .MILLI., .METRE. ) );
#22157 = ORIENTED_EDGE ( 'NONE', *, *, #5498, .T. ) ;
#22158 = AXIS2_PLACEMENT_3D ( 'NONE', #260, #7149, #15928 ) ;
#22159 = EDGE_CURVE ( 'NONE', #18799, #15830, #8397, .T. ) ;
#22160 = LINE ( 'NONE', #19719, #14787 ) ;
#22161 = CARTESIAN_POINT ( 'NONE',  ( -201.7173803564383263, 94.30285377706006500, -30.02230663004699451 ) ) ;
#22162 = ORIENTED_EDGE ( 'NONE', *, *, #12735, .F. ) ;
#22163 = VECTOR ( 'NONE', #4925, 1000.000000000000000 ) ;
#22164 = VERTEX_POINT ( 'NONE', #20158 ) ;
#22165 = DIRECTION ( 'NONE',  ( -0.9985600561963481336, 0.05364526231780537141, 0.000000000000000000 ) ) ;
#22166 = PLANE ( 'NONE',  #21723 ) ;
#22167 = ORIENTED_EDGE ( 'NONE', *, *, #12972, .T. ) ;
#22168 = VERTEX_POINT ( 'NONE', #21886 ) ;
#22169 = CIRCLE ( 'NONE', #16680, 9.999999999999996447 ) ;
#22170 = DIRECTION ( 'NONE',  ( -0.4528218681382909505, -0.8916010070293484135, 0.000000000000000000 ) ) ;
#22171 = EDGE_CURVE ( 'NONE', #25311, #22340, #3816, .T. ) ;
#22172 = AXIS2_PLACEMENT_3D ( 'NONE', #26747, #17555, #4615 ) ;
#22173 = EDGE_CURVE ( 'NONE', #6438, #12064, #6658, .T. ) ;
#22174 = DIRECTION ( 'NONE',  ( -0.000000000000000000, -0.000000000000000000, 1.000000000000000000 ) ) ;
#22175 = DIRECTION ( 'NONE',  ( -0.8916010070297548662, -0.4528218681374907573, 0.000000000000000000 ) ) ;
#22176 = FACE_OUTER_BOUND ( 'NONE', #16202, .T. ) ;
#22177 = CIRCLE ( 'NONE', #4277, 30.00000000000000000 ) ;
#22178 = DIRECTION ( 'NONE',  ( 0.4528218681372309096, -0.8916010070298868717, 0.000000000000000000 ) ) ;
#22179 = CARTESIAN_POINT ( 'NONE',  ( 157.9999999999996874, 269.1575001501400379, 45.00000000000000000 ) ) ;
#22180 = DIRECTION ( 'NONE',  ( -0.000000000000000000, -0.000000000000000000, -1.000000000000000000 ) ) ;
#22181 = ORIENTED_EDGE ( 'NONE', *, *, #20931, .T. ) ;
#22182 = CARTESIAN_POINT ( 'NONE',  ( 158.0000000000015064, 61.00387452705632541, -45.00000000000000000 ) ) ;
#22183 = LINE ( 'NONE', #22328, #11102 ) ;
#22184 = FACE_OUTER_BOUND ( 'NONE', #14401, .T. ) ;
#22185 = CARTESIAN_POINT ( 'NONE',  ( 217.4999999999996305, 133.0668745871126930, -36.86484227207694886 ) ) ;
#22186 = VERTEX_POINT ( 'NONE', #24188 ) ;
#22187 = EDGE_CURVE ( 'NONE', #18495, #11369, #28330, .T. ) ;
#22188 = CARTESIAN_POINT ( 'NONE',  ( 157.4999999999998579, 181.1279373836408411, 45.00000000000000000 ) ) ;
#22189 = ORIENTED_EDGE ( 'NONE', *, *, #16297, .T. ) ;
#22190 = EDGE_CURVE ( 'NONE', #627, #860, #9101, .T. ) ;
#22191 = CARTESIAN_POINT ( 'NONE',  ( 157.4999999999998579, 171.0964373536126573, 45.00000000000000000 ) ) ;
#22192 = LINE ( 'NONE', #16027, #15161 ) ;
#22193 = CARTESIAN_POINT ( 'NONE',  ( 140.6165658301760004, 249.4696452662898025, -147.1195141158909223 ) ) ;
#22194 = ORIENTED_EDGE ( 'NONE', *, *, #16085, .T. ) ;
#22195 = CARTESIAN_POINT ( 'NONE',  ( 157.4999999999998579, 80.81293708335913095, 45.00000000000000000 ) ) ;
#22196 = EDGE_LOOP ( 'NONE', ( #10995, #8975, #15355, #12362 ) ) ;
#22197 = VECTOR ( 'NONE', #17435, 1000.000000000000000 ) ;
#22198 = EDGE_CURVE ( 'NONE', #5015, #21239, #6793, .T. ) ;
#22199 = CARTESIAN_POINT ( 'NONE',  ( 157.4999999999998579, 58.24206201579573872, 45.00000000000000000 ) ) ;
#22200 = ORIENTED_EDGE ( 'NONE', *, *, #18471, .F. ) ;
#22201 = CARTESIAN_POINT ( 'NONE',  ( -268.0706223630187992, -170.6109535803436472, 94.24395792536559213 ) ) ;
#22202 = ORIENTED_EDGE ( 'NONE', *, *, #3175, .T. ) ;
#22203 = ADVANCED_FACE ( 'NONE', ( #11113 ), #4630, .F. ) ;
#22204 = CIRCLE ( 'NONE', #7971, 3.532530335305414493 ) ;
#22205 = EDGE_LOOP ( 'NONE', ( #15065, #2760, #15170, #3462 ) ) ;
#22206 = FACE_OUTER_BOUND ( 'NONE', #6639, .T. ) ;
#22207 = ORIENTED_EDGE ( 'NONE', *, *, #11473, .T. ) ;
#22208 = ORIENTED_EDGE ( 'NONE', *, *, #18406, .T. ) ;
#22209 = VERTEX_POINT ( 'NONE', #13565 ) ;
#22210 = CARTESIAN_POINT ( 'NONE',  ( 95.55652878161114927, 240.7834791927029983, 9.443977278918188389 ) ) ;
#22211 = LINE ( 'NONE', #12898, #26585 ) ;
#22212 = DIRECTION ( 'NONE',  ( -0.000000000000000000, -0.000000000000000000, -1.000000000000000000 ) ) ;
#22213 = AXIS2_PLACEMENT_3D ( 'NONE', #22684, #18230, #16223 ) ;
#22214 = CARTESIAN_POINT ( 'NONE',  ( 187.4999999999996305, 258.6181251126050711, 1.387778780781445676E-14 ) ) ;
#22215 = LINE ( 'NONE', #13185, #28198 ) ;
#22216 = DIRECTION ( 'NONE',  ( -1.000000000000000000, 0.000000000000000000, 0.000000000000000000 ) ) ;
#22217 = FACE_OUTER_BOUND ( 'NONE', #12821, .T. ) ;
#22218 = LINE ( 'NONE', #2523, #13108 ) ;
#22219 = VECTOR ( 'NONE', #15987, 1000.000000000000000 ) ;
#22220 = CARTESIAN_POINT ( 'NONE',  ( 141.9187638636469160, 241.9574749595457774, -45.00000000000000000 ) ) ;
#22221 = CARTESIAN_POINT ( 'NONE',  ( 136.0000000000000853, 196.9999999999997442, -45.00000000000000000 ) ) ;
#22222 = DIRECTION ( 'NONE',  ( 0.8916010070295820045, -0.4528218681378310406, 0.000000000000000000 ) ) ;
#22223 = VERTEX_POINT ( 'NONE', #9246 ) ;
#22224 = DIRECTION ( 'NONE',  ( -0.000000000000000000, -0.000000000000000000, -1.000000000000000000 ) ) ;
#22225 = DIRECTION ( 'NONE',  ( -0.4918581970360879074, 0.000000000000000000, 0.8706753206611571594 ) ) ;
#22226 = CARTESIAN_POINT ( 'NONE',  ( 157.4999999999996589, 278.9350626764145318, 45.00000000000000000 ) ) ;
#22227 = FACE_OUTER_BOUND ( 'NONE', #20651, .T. ) ;
#22228 = ADVANCED_FACE ( 'NONE', ( #26767, #15868, #24616, #8678, #13710 ), #10834, .T. ) ;
#22229 = EDGE_LOOP ( 'NONE', ( #4733, #24682, #7841, #20750 ) ) ;
#22230 = ADVANCED_FACE ( 'NONE', ( #18154 ), #27185, .F. ) ;
#22231 = FACE_OUTER_BOUND ( 'NONE', #2606, .T. ) ;
#22232 = VERTEX_POINT ( 'NONE', #14132 ) ;
#22233 = CARTESIAN_POINT ( 'NONE',  ( -23.16361609519321973, 129.3663660641504407, -15.59648484705163796 ) ) ;
#22234 = ORIENTED_EDGE ( 'NONE', *, *, #2482, .T. ) ;
#22235 = AXIS2_PLACEMENT_3D ( 'NONE', #15121, #16706, #27741 ) ;
#22236 = VERTEX_POINT ( 'NONE', #16561 ) ;
#22237 = VERTEX_POINT ( 'NONE', #26909 ) ;
#22238 = VERTEX_POINT ( 'NONE', #27453 ) ;
#22239 = AXIS2_PLACEMENT_3D ( 'NONE', #8835, #17029, #6115 ) ;
#22240 = ORIENTED_EDGE ( 'NONE', *, *, #10209, .F. ) ;
#22241 = ORIENTED_EDGE ( 'NONE', *, *, #1308, .F. ) ;
#22242 = CARTESIAN_POINT ( 'NONE',  ( 158.0000000000006253, 148.2716247822957882, 45.00000000000000000 ) ) ;
#22243 = DIRECTION ( 'NONE',  ( 0.000000000000000000, 0.000000000000000000, -1.000000000000000000 ) ) ;
#22244 = FACE_OUTER_BOUND ( 'NONE', #6264, .T. ) ;
#22245 = CYLINDRICAL_SURFACE ( 'NONE', #12120, 67.21503689626328537 ) ;
#22246 = CARTESIAN_POINT ( 'NONE',  ( -219.7112380651049364, 60.27397245185820651, 23.81555219817632008 ) ) ;
#22247 = CARTESIAN_POINT ( 'NONE',  ( 147.1752285801744904, 204.1329331941753082, 45.00000000000000000 ) ) ;
#22248 = FACE_OUTER_BOUND ( 'NONE', #13345, .T. ) ;
#22249 = ADVANCED_FACE ( 'NONE', ( #11839 ), #16007, .F. ) ;
#22250 = DIRECTION ( 'NONE',  ( 0.8916010070296327417, -0.4528218681377311761, 0.000000000000000000 ) ) ;
#22251 = CARTESIAN_POINT ( 'NONE',  ( 157.4999999999998579, 75.79718706834503905, 45.00000000000000000 ) ) ;
#22252 = CARTESIAN_POINT ( 'NONE',  ( 232.4999999999996305, 83.06687458711267880, 36.86484227207694175 ) ) ;
#22253 = DIRECTION ( 'NONE',  ( 0.000000000000000000, 0.000000000000000000, -1.000000000000000000 ) ) ;
#22254 = DIRECTION ( 'NONE',  ( -0.000000000000000000, 1.000000000000000000, -1.387778780781445429E-16 ) ) ;
#22255 = VECTOR ( 'NONE', #16534, 999.9999999999998863 ) ;
#22256 = CARTESIAN_POINT ( 'NONE',  ( -0.3498732073529682296, 134.1707435274499005, 15.55713657458744947 ) ) ;
#22257 = CARTESIAN_POINT ( 'NONE',  ( -209.9870476429693156, 61.15597564521014817, 23.95642062441354625 ) ) ;
#22258 = CARTESIAN_POINT ( 'NONE',  ( 153.4775906502255509, 227.6536686473015436, 45.00000000000000000 ) ) ;
#22259 = EDGE_CURVE ( 'NONE', #22407, #24933, #23549, .T. ) ;
#22260 = CARTESIAN_POINT ( 'NONE',  ( 157.9999999999998295, 229.0315000300280417, 45.00000000000000000 ) ) ;
#22261 = VECTOR ( 'NONE', #6217, 1000.000000000000000 ) ;
#22263 = ORIENTED_EDGE ( 'NONE', *, *, #6970, .F. ) ;
#22262 = ORIENTED_EDGE ( 'NONE', *, *, #22717, .T. ) ;
#22264 = PLANE ( 'NONE',  #12838 ) ;
#22265 = EDGE_CURVE ( 'NONE', #8550, #13590, #9675, .T. ) ;
#22266 = EDGE_CURVE ( 'NONE', #17545, #2342, #11702, .T. ) ;
#22267 = LINE ( 'NONE', #20105, #1490 ) ;
#22268 = EDGE_CURVE ( 'NONE', #6741, #18918, #631, .T. ) ;
#22269 = CARTESIAN_POINT ( 'NONE',  ( -204.4655292202942292, 92.00796242303097472, -28.73370588204663889 ) ) ;
#22270 = VERTEX_POINT ( 'NONE', #14270 ) ;
#22271 = VERTEX_POINT ( 'NONE', #18433 ) ;
#22272 = ORIENTED_EDGE ( 'NONE', *, *, #10019, .T. ) ;
#22273 = CARTESIAN_POINT ( 'NONE',  ( 157.9999999999998010, 231.5393750375350237, -45.00000000000000000 ) ) ;
#22274 = CARTESIAN_POINT ( 'NONE',  ( -133.4910656777217355, 128.8270384526469172, 17.15628984000436219 ) ) ;
#22275 = ORIENTED_EDGE ( 'NONE', *, *, #5878, .T. ) ;
#22276 = EDGE_LOOP ( 'NONE', ( #11689, #4089, #27522, #14794 ) ) ;
#22277 = AXIS2_PLACEMENT_3D ( 'NONE', #13287, #28201, #26338 ) ;
#22278 = VECTOR ( 'NONE', #3394, 1000.000000000000000 ) ;
#22279 = DIRECTION ( 'NONE',  ( 1.000000000000000000, 0.000000000000000000, 0.000000000000000000 ) ) ;
#22280 = CARTESIAN_POINT ( 'NONE',  ( -40.40953891503691153, 0.000000000000000000, 99.00000000000000000 ) ) ;
#22281 = ORIENTED_EDGE ( 'NONE', *, *, #19596, .T. ) ;
#22282 = PLANE ( 'NONE',  #23829 ) ;
#22283 = CIRCLE ( 'NONE', #25033, 2.000000000000012879 ) ;
#22284 = DIRECTION ( 'NONE',  ( 1.000000000000000000, 0.000000000000000000, 0.000000000000000000 ) ) ;
#22285 = LINE ( 'NONE', #2594, #2491 ) ;
#22286 = CARTESIAN_POINT ( 'NONE',  ( 157.4999999999998579, 110.9074371734436255, 45.00000000000000000 ) ) ;
#22287 = CARTESIAN_POINT ( 'NONE',  ( -220.5757601432208617, 60.53190028573507675, -22.93231238515986092 ) ) ;
#22288 = EDGE_CURVE ( 'NONE', #17959, #15548, #14001, .T. ) ;
#22289 = EDGE_CURVE ( 'NONE', #21270, #6129, #16425, .T. ) ;
#22290 = VERTEX_POINT ( 'NONE', #25314 ) ;
#22291 = DIRECTION ( 'NONE',  ( -1.000000000000000000, 0.000000000000000000, 0.000000000000000000 ) ) ;
#22292 = ADVANCED_FACE ( 'NONE', ( #3330 ), #11560, .F. ) ;
#22293 = AXIS2_PLACEMENT_3D ( 'NONE', #9755, #18788, #7313 ) ;
#22294 = CARTESIAN_POINT ( 'NONE',  ( -221.1044245926502185, 138.9463871349811939, -14.97905406095822656 ) ) ;
#22295 = DIRECTION ( 'NONE',  ( 0.000000000000000000, 1.000000000000000000, -0.000000000000000000 ) ) ;
#22296 = ORIENTED_EDGE ( 'NONE', *, *, #16385, .F. ) ;
#22297 = VECTOR ( 'NONE', #23193, 1000.000000000000000 ) ;
#22298 = PLANE ( 'NONE',  #11474 ) ;
#22299 = EDGE_CURVE ( 'NONE', #23503, #7481, #20865, .T. ) ;
#22300 = CARTESIAN_POINT ( 'NONE',  ( -180.0000000000000284, -40.00000000000004974, 70.00000000000001421 ) ) ;
#22301 = CARTESIAN_POINT ( 'NONE',  ( -141.1970735032543303, 70.84982942354511692, 82.84771202320575867 ) ) ;
#22302 = ORIENTED_EDGE ( 'NONE', *, *, #23134, .T. ) ;
#22303 = CARTESIAN_POINT ( 'NONE',  ( 0.000000000000000000, 0.000000000000000000, 0.000000000000000000 ) ) ;
#22304 = AXIS2_PLACEMENT_3D ( 'NONE', #14555, #12547, #3757 ) ;
#22305 = ORIENTED_EDGE ( 'NONE', *, *, #18568, .T. ) ;
#22306 = EDGE_CURVE ( 'NONE', #1362, #15527, #27046, .T. ) ;
#22307 = DIRECTION ( 'NONE',  ( -1.541976423090495387E-16, 1.000000000000000000, 0.000000000000000000 ) ) ;
#22308 = LINE ( 'NONE', #11829, #6231 ) ;
#22309 = ORIENTED_EDGE ( 'NONE', *, *, #14984, .T. ) ;
#22310 = ORIENTED_EDGE ( 'NONE', *, *, #15888, .F. ) ;
#22311 = CARTESIAN_POINT ( 'NONE',  ( 158.0000000000004547, 165.8267498348450886, -45.00000000000000000 ) ) ;
#22312 = CARTESIAN_POINT ( 'NONE',  ( 157.4999999999998579, 193.6673124211760353, 45.00000000000000000 ) ) ;
#22313 = ORIENTED_EDGE ( 'NONE', *, *, #22789, .T. ) ;
#22314 = CARTESIAN_POINT ( 'NONE',  ( 157.4999999999996589, 281.4429376839215138, -45.00000000000000000 ) ) ;
#22315 = ORIENTED_EDGE ( 'NONE', *, *, #10353, .F. ) ;
#22316 = VECTOR ( 'NONE', #15253, 1000.000000000000000 ) ;
#22317 = CARTESIAN_POINT ( 'NONE',  ( -31.67953875179438228, 128.0283279034048007, 17.49215224234154675 ) ) ;
#22318 = CARTESIAN_POINT ( 'NONE',  ( 158.0000000000013642, 78.05112457209858690, -45.00000000000000000 ) ) ;
#22319 = CARTESIAN_POINT ( 'NONE',  ( 158.0000000000010516, 103.6377496546760568, 45.00000000000000000 ) ) ;
#22320 = CARTESIAN_POINT ( 'NONE',  ( -31.66438925218564293, 128.0276125918315131, -17.49246453772925847 ) ) ;
#22321 = VECTOR ( 'NONE', #20630, 1000.000000000000114 ) ;
#22322 = CARTESIAN_POINT ( 'NONE',  ( 113.0425250404539241, 213.0812361363525440, 45.00000000000000000 ) ) ;
#22323 = FACE_OUTER_BOUND ( 'NONE', #12387, .T. ) ;
#22324 = CYLINDRICAL_SURFACE ( 'NONE', #18883, 19.07743405327024888 ) ;
#22325 = EDGE_CURVE ( 'NONE', #15954, #14251, #14410, .T. ) ;
#22326 = ORIENTED_EDGE ( 'NONE', *, *, #3642, .T. ) ;
#22327 = DIRECTION ( 'NONE',  ( -0.000000000000000000, -0.000000000000000000, -1.000000000000000000 ) ) ;
#22328 = CARTESIAN_POINT ( 'NONE',  ( 157.4999999999998579, 78.30506207585207790, 45.00000000000000000 ) ) ;
#22329 = CARTESIAN_POINT ( 'NONE',  ( -12.24491960465745599, -23.01420295945612082, 95.00000000000000000 ) ) ;
#22330 = DIRECTION ( 'NONE',  ( -0.000000000000000000, -0.000000000000000000, 1.000000000000000000 ) ) ;
#22331 = VERTEX_POINT ( 'NONE', #9396 ) ;
#22332 = CARTESIAN_POINT ( 'NONE',  ( -218.0684950290401787, 60.60891383183042080, 12.02124378490089285 ) ) ;
#22333 = VERTEX_POINT ( 'NONE', #22881 ) ;
#22334 = CARTESIAN_POINT ( 'NONE',  ( 187.4999999999996305, 288.9665627064425166, 45.00000000000000000 ) ) ;
#22335 = DIRECTION ( 'NONE',  ( 0.000000000000000000, 0.000000000000000000, -1.000000000000000000 ) ) ;
#22336 = CARTESIAN_POINT ( 'NONE',  ( 137.6643377305021261, 249.8836732857602669, -150.3903514073973611 ) ) ;
#22337 = ORIENTED_EDGE ( 'NONE', *, *, #16066, .F. ) ;
#22338 = DIRECTION ( 'NONE',  ( -0.000000000000000000, -0.000000000000000000, -1.000000000000000000 ) ) ;
#22339 = DIRECTION ( 'NONE',  ( -0.000000000000000000, -0.3247168404252948060, -0.9458112779747414045 ) ) ;
#22340 = VERTEX_POINT ( 'NONE', #3189 ) ;
#22341 = AXIS2_PLACEMENT_3D ( 'NONE', #625, #18424, #9390 ) ;
#22342 = EDGE_CURVE ( 'NONE', #23124, #27860, #11978, .T. ) ;
#22343 = CARTESIAN_POINT ( 'NONE',  ( -215.1490939589890274, 71.74855184469089409, 26.39437962326677578 ) ) ;
#22344 = EDGE_LOOP ( 'NONE', ( #14544, #4447, #12248, #3567 ) ) ;
#22345 = EDGE_CURVE ( 'NONE', #17770, #19699, #20719, .T. ) ;
#22346 = CARTESIAN_POINT ( 'NONE',  ( -17.24491960465746132, 75.97823757117562593, 95.00000000000000000 ) ) ;
#22347 = ORIENTED_EDGE ( 'NONE', *, *, #27910, .T. ) ;
#22348 = ORIENTED_EDGE ( 'NONE', *, *, #12318, .T. ) ;
#22349 = LINE ( 'NONE', #27629, #19564 ) ;
#22350 = VERTEX_POINT ( 'NONE', #5212 ) ;
#22351 = EDGE_LOOP ( 'NONE', ( #320, #26109, #14286, #19817 ) ) ;
#22352 = ORIENTED_EDGE ( 'NONE', *, *, #19113, .T. ) ;
#22353 = EDGE_CURVE ( 'NONE', #24201, #11803, #16665, .T. ) ;
#22354 = CARTESIAN_POINT ( 'NONE',  ( 106.3805259670891559, 243.6561646000983785, 30.69292865458877273 ) ) ;
#22355 = B_SPLINE_CURVE_WITH_KNOTS ( 'NONE', 3,
 ( #5264, #14049, #22799, #3097, #11891, #25223, #26063, #17166, #8555, #17023, #13020, #1514, #12732, #27923, #25779, #10848, #8270, #4088, #28066, #26203, #10564, #19605, #12594, #14738 ),
 .UNSPECIFIED., .F., .F.,
 ( 4, 2, 2, 2, 2, 2, 2, 2, 2, 2, 2, 4 ),
 ( 0.006955041467238867736, 0.01003080572916798148, 0.01156868786013253748, 0.01310656999109709522, 0.01618233425302619682, 0.01772021638399075283, 0.01925809851495530883, 0.02233386277688433411, 0.02387174490784884848, 0.02540962703881335938, 0.02848539130074245404, 0.03156115556267154870 ),
 .UNSPECIFIED. ) ;
#22356 = ADVANCED_FACE ( 'NONE', ( #10094 ), #10516, .F. ) ;
#22357 = CYLINDRICAL_SURFACE ( 'NONE', #12412, 6.000000000000032863 ) ;
#22358 = AXIS2_PLACEMENT_3D ( 'NONE', #1315, #25578, #25164 ) ;
#22359 = CLOSED_SHELL ( 'NONE', ( #23895, #8664, #11939, #24925, #1846, #8709, #15037, #11412, #6142, #21108, #22030, #14124, #168, #5133, #11515, #2878, #6155, #26249, #12881, #23934, #24502, #16748, #18538, #4025, #18275, #5872, #19504, #7711, #7379, #4614, #20642, #10601, #17171, #9698, #21745, #8382, #18681, #23387 ) ) ;
#22360 = DIRECTION ( 'NONE',  ( 1.000000000000000000, 0.000000000000000000, 0.000000000000000000 ) ) ;
#22361 = CARTESIAN_POINT ( 'NONE',  ( 157.4999999999998579, 141.0019372635281627, 45.00000000000000000 ) ) ;
#22362 = DIRECTION ( 'NONE',  ( 0.000000000000000000, -0.000000000000000000, -1.000000000000000000 ) ) ;
#22363 = DIRECTION ( 'NONE',  ( 0.000000000000000000, 0.000000000000000000, -1.000000000000000000 ) ) ;
#22364 = CARTESIAN_POINT ( 'NONE',  ( 158.0000000000005116, 160.8109998198309825, -45.00000000000000000 ) ) ;
#22365 = LINE ( 'NONE', #2672, #17492 ) ;
#22366 = DIRECTION ( 'NONE',  ( -1.000000000000000000, -0.000000000000000000, -0.000000000000000000 ) ) ;
#22367 = DIRECTION ( 'NONE',  ( 0.2066290158914539099, -0.9784193629480814058, 0.000000000000000000 ) ) ;
#22368 = ORIENTED_EDGE ( 'NONE', *, *, #25003, .F. ) ;
#22369 = CARTESIAN_POINT ( 'NONE',  ( 89.99999999999988631, 240.0000000000000284, 6.270166537925822681 ) ) ;
#22370 = PLANE ( 'NONE',  #16516 ) ;
#22371 = DIRECTION ( 'NONE',  ( -0.5457381880580733924, -0.8379557447115514313, 0.000000000000000000 ) ) ;
#22372 = DIRECTION ( 'NONE',  ( 0.4528218681375507093, -0.8916010070297244461, 0.000000000000000000 ) ) ;
#22373 = ORIENTED_EDGE ( 'NONE', *, *, #25090, .T. ) ;
#22374 = VECTOR ( 'NONE', #22430, 1000.000000000000114 ) ;
#22375 = EDGE_CURVE ( 'NONE', #2585, #23830, #7932, .T. ) ;
#22376 = CARTESIAN_POINT ( 'NONE',  ( 2.399999999999999911, 1.249999999999999556, 7.582700855991164168 ) ) ;
#22377 = EDGE_LOOP ( 'NONE', ( #27383, #5501, #16285, #19518, #10928, #26714, #5562, #27136 ) ) ;
#22378 = DIRECTION ( 'NONE',  ( -1.000000000000000000, 0.000000000000000000, 0.000000000000000000 ) ) ;
#22379 = VECTOR ( 'NONE', #12649, 1000.000000000000227 ) ;
#22380 = VERTEX_POINT ( 'NONE', #3473 ) ;
#22381 = ORIENTED_EDGE ( 'NONE', *, *, #19549, .F. ) ;
#22382 = VERTEX_POINT ( 'NONE', #8362 ) ;
#22383 = VERTEX_POINT ( 'NONE', #1878 ) ;
#22384 = CARTESIAN_POINT ( 'NONE',  ( 157.4999999999998579, 120.9389372034718093, -45.00000000000000000 ) ) ;
#22385 = FACE_OUTER_BOUND ( 'NONE', #1106, .T. ) ;
#22386 = CARTESIAN_POINT ( 'NONE',  ( 157.4999999999998579, 176.1121873686267350, 45.00000000000000000 ) ) ;
#22387 = FACE_BOUND ( 'NONE', #25970, .T. ) ;
#22388 = ADVANCED_FACE ( 'NONE', ( #12264 ), #3752, .T. ) ;
#22389 = DIRECTION ( 'NONE',  ( 0.000000000000000000, 0.000000000000000000, 1.000000000000000000 ) ) ;
#22390 = EDGE_CURVE ( 'NONE', #17645, #12991, #6058, .T. ) ;
#22391 = CARTESIAN_POINT ( 'NONE',  ( -228.3003245610658496, 63.46411924056219789, 17.58993856060416405 ) ) ;
#22393 = CARTESIAN_POINT ( 'NONE',  ( 158.0000000000010800, 103.1298746471690038, 45.00000000000000000 ) ) ;
#22392 = VECTOR ( 'NONE', #13083, 1000.000000000000227 ) ;
#22394 = DIRECTION ( 'NONE',  ( 1.000000000000000000, 0.000000000000000000, 0.000000000000000000 ) ) ;
#22395 = CARTESIAN_POINT ( 'NONE',  ( -3.642919299551294898E-14, 139.9999999999999716, -45.00000000000000000 ) ) ;
#22396 = CIRCLE ( 'NONE', #4059, 562.1290781602206152 ) ;
#22397 = DIRECTION ( 'NONE',  ( 0.4528218681382713551, -0.8916010070293584056, 0.000000000000000000 ) ) ;
#22398 = ADVANCED_FACE ( 'NONE', ( #26015 ), #23589, .T. ) ;
#22399 = CARTESIAN_POINT ( 'NONE',  ( -42.99650729631200363, 71.03850157808263077, 99.00000000000000000 ) ) ;
#22400 = DIRECTION ( 'NONE',  ( -0.000000000000000000, -1.000000000000000000, -0.000000000000000000 ) ) ;
#22401 = CARTESIAN_POINT ( 'NONE',  ( 93.17300876009500143, -24.96563245364655259, 45.00000000000000000 ) ) ;
#22402 = LINE ( 'NONE', #11502, #23802 ) ;
#22403 = DIRECTION ( 'NONE',  ( -0.000000000000000000, 1.000000000000000000, 0.000000000000000000 ) ) ;
#22404 = DIRECTION ( 'NONE',  ( -0.000000000000000000, -0.000000000000000000, -1.000000000000000000 ) ) ;
#22405 = PLANE ( 'NONE',  #17553 ) ;
#22407 = VERTEX_POINT ( 'NONE', #14837 ) ;
#22406 = VERTEX_POINT ( 'NONE', #10374 ) ;
#22408 = DIRECTION ( 'NONE',  ( 0.000000000000000000, 1.000000000000000000, 0.000000000000000000 ) ) ;
#22409 = PRESENTATION_LAYER_ASSIGNMENT (  '', '', ( #21535 ) ) ;
#22410 = CARTESIAN_POINT ( 'NONE',  ( 232.4749999999995964, 133.0668745871126930, -36.86484227207694886 ) ) ;
#22411 = ORIENTED_EDGE ( 'NONE', *, *, #11275, .T. ) ;
#22412 = ORIENTED_EDGE ( 'NONE', *, *, #5312, .T. ) ;
#22413 = ORIENTED_EDGE ( 'NONE', *, *, #11374, .T. ) ;
#22414 = VECTOR ( 'NONE', #818, 1000.000000000000114 ) ;
#22415 = CARTESIAN_POINT ( 'NONE',  ( 134.6436608991879496, 206.7391133850113079, 45.00000000000000000 ) ) ;
#22416 = CARTESIAN_POINT ( 'NONE',  ( 157.4999999999998010, 238.8090625563025071, 45.00000000000000000 ) ) ;
#22417 = CIRCLE ( 'NONE', #16917, 18.91107291867258411 ) ;
#22418 = ORIENTED_EDGE ( 'NONE', *, *, #7465, .F. ) ;
#22419 = VERTEX_POINT ( 'NONE', #18847 ) ;
#22420 = CARTESIAN_POINT ( 'NONE',  ( 158.0000000000016769, 47.95662448201407102, -45.00000000000000000 ) ) ;
#22421 = CARTESIAN_POINT ( 'NONE',  ( 134.9999999999998579, 220.0000000000000284, 90.00000000000002842 ) ) ;
#22422 = ORIENTED_EDGE ( 'NONE', *, *, #2763, .T. ) ;
#22423 = EDGE_CURVE ( 'NONE', #27590, #26144, #21426, .T. ) ;
#22424 = CARTESIAN_POINT ( 'NONE',  ( -206.1401686320352837, 90.30263034637913222, 28.11534395024635558 ) ) ;
#22425 = CARTESIAN_POINT ( 'NONE',  ( 157.4999999999998579, 138.4940622560211239, 45.00000000000000000 ) ) ;
#22426 = EDGE_CURVE ( 'NONE', #24580, #16161, #26291, .T. ) ;
#22427 = CONICAL_SURFACE ( 'NONE', #26530, 6.025000000000002132, 0.7853981633974482790 ) ;
#22428 = ADVANCED_FACE ( 'NONE', ( #27595 ), #14549, .F. ) ;
#22429 = CARTESIAN_POINT ( 'NONE',  ( -187.8924994060663494, 156.4650759647683742, -15.00000000000000000 ) ) ;
#22430 = DIRECTION ( 'NONE',  ( -0.8916010070293409751, -0.4528218681383056610, 0.000000000000000000 ) ) ;
#22431 = CARTESIAN_POINT ( 'NONE',  ( -208.8418814728804023, 74.65865074066952900, -37.27912060900214186 ) ) ;
#22432 = AXIS2_PLACEMENT_3D ( 'NONE', #15311, #8554, #14886 ) ;
#22433 = EDGE_LOOP ( 'NONE', ( #2864, #24181, #16515, #7751 ) ) ;
#22434 = LINE ( 'NONE', #2743, #19676 ) ;
#22435 = AXIS2_PLACEMENT_3D ( 'NONE', #12236, #1430, #8045 ) ;
#22436 = DIRECTION ( 'NONE',  ( -0.8660254037844362651, 0.5000000000000039968, -0.000000000000000000 ) ) ;
#22437 = DIRECTION ( 'NONE',  ( 0.8916010070296531698, -0.4528218681376911525, 0.000000000000000000 ) ) ;
#22438 = DIRECTION ( 'NONE',  ( -0.000000000000000000, -0.000000000000000000, 1.000000000000000000 ) ) ;
#22439 = ORIENTED_EDGE ( 'NONE', *, *, #24297, .F. ) ;
#22440 = DIRECTION ( 'NONE',  ( 0.000000000000000000, 0.000000000000000000, 1.000000000000000000 ) ) ;
#22441 = CARTESIAN_POINT ( 'NONE',  ( -233.4632575733469650, 77.89441575049642097, 15.30815287833161342 ) ) ;
#22442 = LINE ( 'NONE', #2609, #15861 ) ;
#22443 = ORIENTED_EDGE ( 'NONE', *, *, #7483, .T. ) ;
#22444 = SHAPE_REPRESENTATION_RELATIONSHIP ( 'NONE' , 'NONE' ,  #10277, #27021 ) ;
#22445 = EDGE_LOOP ( 'NONE', ( #16075, #20962, #25714 ) ) ;
#22446 = DIRECTION ( 'NONE',  ( 1.000000000000000000, 0.000000000000000000, 0.000000000000000000 ) ) ;
#22447 = AXIS2_PLACEMENT_3D ( 'NONE', #8830, #19887, #11283 ) ;
#22448 = CARTESIAN_POINT ( 'NONE',  ( 209.9999999999999432, -280.0000000000000000, -99.99999999999995737 ) ) ;
#22449 = ORIENTED_EDGE ( 'NONE', *, *, #15720, .T. ) ;
#22450 = PRESENTATION_LAYER_ASSIGNMENT (  '', '', ( #2715 ) ) ;
#22451 = VERTEX_POINT ( 'NONE', #25876 ) ;
#22452 = CARTESIAN_POINT ( 'NONE',  ( 157.9999999999997726, 243.5708750675630370, 45.00000000000000000 ) ) ;
#22453 = AXIS2_PLACEMENT_3D ( 'NONE', #25540, #21090, #1270 ) ;
#22454 = EDGE_CURVE ( 'NONE', #23614, #27147, #25731, .T. ) ;
#22455 = DIRECTION ( 'NONE',  ( 0.4528218681375707488, -0.8916010070297142320, 0.000000000000000000 ) ) ;
#22456 = ORIENTED_EDGE ( 'NONE', *, *, #13077, .T. ) ;
#22457 = DIRECTION ( 'NONE',  ( 0.4528218681374108767, -0.8916010070297955004, 0.000000000000000000 ) ) ;
#22458 = ORIENTED_EDGE ( 'NONE', *, *, #5671, .T. ) ;
#22459 = CARTESIAN_POINT ( 'NONE',  ( -6.823563161442123715, 131.5377459308396055, 16.21528367945318649 ) ) ;
#22460 = CIRCLE ( 'NONE', #10074, 3.532530335305414493 ) ;
#22461 = ADVANCED_FACE ( 'NONE', ( #17121 ), #6201, .F. ) ;
#22462 = EDGE_CURVE ( 'NONE', #24936, #17385, #22169, .T. ) ;
#22463 = LINE ( 'NONE', #11414, #5293 ) ;
#22464 = DIRECTION ( 'NONE',  ( -0.000000000000000000, 1.000000000000000000, -0.000000000000000000 ) ) ;
#22465 = CARTESIAN_POINT ( 'NONE',  ( -23.58081250372386251, 128.1194696888447311, -17.45268724460935061 ) ) ;
#22466 = CARTESIAN_POINT ( 'NONE',  ( -124.9781469243918934, 222.2250949724356985, 5.000000000000002665 ) ) ;
#22467 = DIRECTION ( 'NONE',  ( -0.5555587585212703461, -0.8314772792026879911, 1.927481641382755247E-15 ) ) ;
#22468 = CARTESIAN_POINT ( 'NONE',  ( 134.9999999999998579, 220.0000000000000284, 84.99999999999995737 ) ) ;
#22469 = ORIENTED_EDGE ( 'NONE', *, *, #17747, .F. ) ;
#22470 = VECTOR ( 'NONE', #13261, 1000.000000000000000 ) ;
#22471 = LINE ( 'NONE', #24910, #25597 ) ;
#22472 = DIRECTION ( 'NONE',  ( 0.000000000000000000, -1.000000000000000000, 0.000000000000000000 ) ) ;
#22473 = CARTESIAN_POINT ( 'NONE',  ( 157.4999999999998579, 151.0334372935563465, -45.00000000000000000 ) ) ;
#22474 = LINE ( 'NONE', #4644, #1101 ) ;
#22475 = EDGE_LOOP ( 'NONE', ( #27437, #13200, #25434, #24355 ) ) ;
#22476 = CARTESIAN_POINT ( 'NONE',  ( 65.00000000000000000, -120.0000000000000711, 63.97500000000001563 ) ) ;
#22477 = AXIS2_PLACEMENT_3D ( 'NONE', #18067, #4687, #13474 ) ;
#22478 = ORIENTED_EDGE ( 'NONE', *, *, #15495, .F. ) ;
#22479 = CARTESIAN_POINT ( 'NONE',  ( -175.0000000000000000, -150.0000000000000853, -69.99999999999998579 ) ) ;
#22480 = DIRECTION ( 'NONE',  ( 0.000000000000000000, 0.000000000000000000, -1.000000000000000000 ) ) ;
#22481 = CARTESIAN_POINT ( 'NONE',  ( -210.0000000000000284, -3.238150488490040751E-14, 100.0000000000000142 ) ) ;
#22482 = ORIENTED_EDGE ( 'NONE', *, *, #3800, .F. ) ;
#22483 =( NAMED_UNIT ( * ) PLANE_ANGLE_UNIT ( ) SI_UNIT ( $, .RADIAN. ) );
#22484 = SURFACE_STYLE_FILL_AREA ( #2791 ) ;
#22485 = VERTEX_POINT ( 'NONE', #10236 ) ;
#22486 = LINE ( 'NONE', #931, #7492 ) ;
#22487 = ORIENTED_EDGE ( 'NONE', *, *, #6265, .T. ) ;
#22488 = CARTESIAN_POINT ( 'NONE',  ( 157.9999999999998295, 226.5236250225210313, 45.00000000000000000 ) ) ;
#22489 = ORIENTED_EDGE ( 'NONE', *, *, #52, .T. ) ;
#22490 = EDGE_CURVE ( 'NONE', #10018, #17075, #6336, .T. ) ;
#22491 = ORIENTED_EDGE ( 'NONE', *, *, #21986, .F. ) ;
#22492 = DIRECTION ( 'NONE',  ( -0.000000000000000000, -0.000000000000000000, -1.000000000000000000 ) ) ;
#22493 = ORIENTED_EDGE ( 'NONE', *, *, #23878, .F. ) ;
#22494 = ADVANCED_FACE ( 'NONE', ( #1604 ), #25392, .T. ) ;
#22495 = VECTOR ( 'NONE', #27358, 1000.000000000000000 ) ;
#22496 = VERTEX_POINT ( 'NONE', #19130 ) ;
#22497 = B_SPLINE_CURVE_WITH_KNOTS ( 'NONE', 3,
 ( #26895, #8941, #11247, #9085, #13697, #15559, #9230, #22301, #17842, #15422, #2462, #17700, #15704, #328 ),
 .UNSPECIFIED., .F., .F.,
 ( 4, 2, 2, 2, 2, 2, 4 ),
 ( 0.000000000000000000, 0.001449387442315872411, 0.002174081163473810027, 0.002898774884631747425, 0.003623468605789684823, 0.004348162326947622655, 0.005797549769263428930 ),
 .UNSPECIFIED. ) ;
#22498 = VERTEX_POINT ( 'NONE', #27872 ) ;
#22499 = CARTESIAN_POINT ( 'NONE',  ( 107.7348956500412100, 246.7603209947075982, 33.46154240484374043 ) ) ;
#22500 = AXIS2_PLACEMENT_3D ( 'NONE', #16532, #19100, #14653 ) ;
#22501 = EDGE_CURVE ( 'NONE', #3649, #14719, #8216, .T. ) ;
#22502 = VECTOR ( 'NONE', #10244, 1000.000000000000114 ) ;
#22503 = DIRECTION ( 'NONE',  ( 0.000000000000000000, 0.000000000000000000, -1.000000000000000000 ) ) ;
#22504 = LINE ( 'NONE', #16190, #26149 ) ;
#22505 = LINE ( 'NONE', #25081, #16543 ) ;
#22506 = DIRECTION ( 'NONE',  ( -0.6681556583950049033, 0.7440215159219103480, 0.000000000000000000 ) ) ;
#22507 = DIRECTION ( 'NONE',  ( -0.000000000000000000, 0.000000000000000000, -1.000000000000000000 ) ) ;
#22508 = EDGE_CURVE ( 'NONE', #8798, #4392, #8645, .T. ) ;
#22509 = CARTESIAN_POINT ( 'NONE',  ( 134.9999999999998579, 220.0000000000000284, -105.0000000000000284 ) ) ;
#22510 = DIRECTION ( 'NONE',  ( 1.000000000000000000, 0.000000000000000000, -0.000000000000000000 ) ) ;
#22511 = DIRECTION ( 'NONE',  ( 0.000000000000000000, 0.000000000000000000, -1.000000000000000000 ) ) ;
#22512 = LINE ( 'NONE', #19920, #21482 ) ;
#22513 = LINE ( 'NONE', #26819, #23091 ) ;
#22514 = ORIENTED_EDGE ( 'NONE', *, *, #12455, .F. ) ;
#22515 = DIRECTION ( 'NONE',  ( -0.000000000000000000, -0.000000000000000000, -1.000000000000000000 ) ) ;
#22516 = CIRCLE ( 'NONE', #20660, 30.00000000000001421 ) ;
#22517 = DIRECTION ( 'NONE',  ( 1.000000000000000000, 0.000000000000000000, 0.000000000000000000 ) ) ;
#22518 = CARTESIAN_POINT ( 'NONE',  ( -210.0000000000000568, -157.0000000000000284, -110.0000000000000284 ) ) ;
#22519 = FACE_OUTER_BOUND ( 'NONE', #2458, .T. ) ;
#22520 = ORIENTED_EDGE ( 'NONE', *, *, #946, .T. ) ;
#22521 = EDGE_CURVE ( 'NONE', #24784, #27410, #2165, .T. ) ;
#22522 = AXIS2_PLACEMENT_3D ( 'NONE', #28381, #19778, #2529 ) ;
#22523 = CARTESIAN_POINT ( 'NONE',  ( 109.9999999999998863, 259.2933449741933032, -44.14322629332889392 ) ) ;
#22524 = EDGE_LOOP ( 'NONE', ( #13958, #6649, #27450, #6780 ) ) ;
#22525 =( NAMED_UNIT ( * ) SI_UNIT ( $, .STERADIAN. ) SOLID_ANGLE_UNIT ( ) );
#22526 = ORIENTED_EDGE ( 'NONE', *, *, #11236, .F. ) ;
#22527 = EDGE_CURVE ( 'NONE', #17008, #23616, #455, .T. ) ;
#22528 = ORIENTED_EDGE ( 'NONE', *, *, #28105, .F. ) ;
#22529 = ORIENTED_EDGE ( 'NONE', *, *, #8651, .F. ) ;
#22530 = ORIENTED_EDGE ( 'NONE', *, *, #26592, .F. ) ;
#22531 = CARTESIAN_POINT ( 'NONE',  ( -134.0122209785728273, 130.0131674746676538, 15.29879588572737426 ) ) ;
#22532 = LINE ( 'NONE', #16080, #4007 ) ;
#22533 = PLANE ( 'NONE',  #2876 ) ;
#22534 = CARTESIAN_POINT ( 'NONE',  ( -100.3750459336811787, 135.9165849456836384, -15.23352683708864141 ) ) ;
#22535 = CARTESIAN_POINT ( 'NONE',  ( 158.0000000000002842, 178.8739998798873216, 45.00000000000000000 ) ) ;
#22536 = ADVANCED_FACE ( 'NONE', ( #26160 ), #24160, .F. ) ;
#22537 = AXIS2_PLACEMENT_3D ( 'NONE', #5329, #27161, #7497 ) ;
#22538 = CARTESIAN_POINT ( 'NONE',  ( -194.2306746384193730, 63.21821459927384979, 44.70951427402087575 ) ) ;
#22539 = DIRECTION ( 'NONE',  ( 0.000000000000000000, -1.000000000000000000, -1.214306433183764966E-16 ) ) ;
#22540 = LINE ( 'NONE', #3410, #10830 ) ;
#22541 = EDGE_CURVE ( 'NONE', #21665, #13456, #4459, .T. ) ;
#22542 = DIRECTION ( 'NONE',  ( 0.000000000000000000, 0.000000000000000000, 1.000000000000000000 ) ) ;
#22543 = CARTESIAN_POINT ( 'NONE',  ( -231.9378824387731299, 93.53122965655668963, -13.00000000000000000 ) ) ;
#22544 = CARTESIAN_POINT ( 'NONE',  ( -68.57415822541635464, 29.64876300893806516, 95.00000000000000000 ) ) ;
#22545 = DIRECTION ( 'NONE',  ( 1.000000000000000000, -0.000000000000000000, -0.000000000000000000 ) ) ;
#22546 = DIRECTION ( 'NONE',  ( 0.000000000000000000, 0.000000000000000000, -1.000000000000000000 ) ) ;
#22547 = CARTESIAN_POINT ( 'NONE',  ( 1.671497233361736612, 135.1829325683629577, 15.36772416567834476 ) ) ;
#22548 = DIRECTION ( 'NONE',  ( -0.9659258262890662028, 0.2588190451025286221, 0.000000000000000000 ) ) ;
#22549 = CARTESIAN_POINT ( 'NONE',  ( 157.4999999999998579, 58.24206201579573872, 45.00000000000000000 ) ) ;
#22550 = CARTESIAN_POINT ( 'NONE',  ( 157.9999999999998579, 221.5078750075070104, 45.00000000000000000 ) ) ;
#22552 = ORIENTED_EDGE ( 'NONE', *, *, #9140, .T. ) ;
#22551 = ORIENTED_EDGE ( 'NONE', *, *, #12060, .F. ) ;
#22553 = ADVANCED_FACE ( 'NONE', ( #11377 ), #3362, .F. ) ;
#22554 = CARTESIAN_POINT ( 'NONE',  ( -146.6428522700808230, 22.24192588826928585, 83.00000000000001421 ) ) ;
#22555 = VECTOR ( 'NONE', #4968, 1000.000000000000114 ) ;
#22556 = PLANE ( 'NONE',  #27179 ) ;
#22557 = ORIENTED_EDGE ( 'NONE', *, *, #18393, .T. ) ;
#22558 = EDGE_LOOP ( 'NONE', ( #16357, #7965, #754, #6935 ) ) ;
#22559 = VECTOR ( 'NONE', #21020, 999.9999999999998863 ) ;
#22561 = EDGE_CURVE ( 'NONE', #5556, #13208, #9215, .T. ) ;
#22560 = ORIENTED_EDGE ( 'NONE', *, *, #2518, .F. ) ;
#22562 = AXIS2_PLACEMENT_3D ( 'NONE', #16927, #25682, #8595 ) ;
#22563 = DIRECTION ( 'NONE',  ( -0.8660254037844363761, 0.5000000000000039968, -0.000000000000000000 ) ) ;
#22564 = CARTESIAN_POINT ( 'NONE',  ( -141.8785761468075464, 126.4564228109756101, 18.21987071921232371 ) ) ;
#22565 = VERTEX_POINT ( 'NONE', #19840 ) ;
#22566 = EDGE_CURVE ( 'NONE', #17603, #27215, #21263, .T. ) ;
#22567 = EDGE_LOOP ( 'NONE', ( #577, #22779, #1983, #14668 ) ) ;
#22568 = PLANE ( 'NONE',  #23396 ) ;
#22569 = PLANE ( 'NONE',  #7684 ) ;
#22570 = LINE ( 'NONE', #14239, #16941 ) ;
#22571 = ORIENTED_EDGE ( 'NONE', *, *, #16385, .T. ) ;
#22572 = CARTESIAN_POINT ( 'NONE',  ( -204.2340599944510586, 92.18449363278668329, 28.15791701117214529 ) ) ;
#22573 = DIRECTION ( 'NONE',  ( 0.8916010070294800860, -0.4528218681380314359, 0.000000000000000000 ) ) ;
#22574 = AXIS2_PLACEMENT_3D ( 'NONE', #9257, #8825, #26342 ) ;
#22575 = CARTESIAN_POINT ( 'NONE',  ( 158.0000000000013927, 73.54324956459154805, 45.00000000000000000 ) ) ;
#22576 = AXIS2_PLACEMENT_3D ( 'NONE', #20851, #22446, #3039 ) ;
#22577 = FACE_OUTER_BOUND ( 'NONE', #16378, .T. ) ;
#22578 = PRODUCT_DEFINITION_FORMATION_WITH_SPECIFIED_SOURCE ( 'ANY', '', #19210, .NOT_KNOWN. ) ;
#22579 = CARTESIAN_POINT ( 'NONE',  ( -215.5934637701523684, 59.01440814108518396, -29.65465734991407132 ) ) ;
#22580 = VECTOR ( 'NONE', #26212, 1000.000000000000000 ) ;
#22581 = LINE ( 'NONE', #2891, #7300 ) ;
#22582 = CARTESIAN_POINT ( 'NONE',  ( -217.7546030100656083, 138.5587306369264411, -15.07876772301851354 ) ) ;
#22583 = LINE ( 'NONE', #11681, #6074 ) ;
#22584 = CARTESIAN_POINT ( 'NONE',  ( 158.0000000000005116, 160.8109998198309825, 45.00000000000000000 ) ) ;
#22585 = ORIENTED_EDGE ( 'NONE', *, *, #5559, .T. ) ;
#22586 = CARTESIAN_POINT ( 'NONE',  ( 267.4999999999996021, 194.4107529906318064, 288.0938197134494203 ) ) ;
#22587 = DIRECTION ( 'NONE',  ( 0.000000000000000000, 9.251858538542967883E-17, -1.000000000000000000 ) ) ;
#22588 = CARTESIAN_POINT ( 'NONE',  ( 157.9999999999996589, 273.6653751576470768, -45.00000000000000000 ) ) ;
#22589 = EDGE_LOOP ( 'NONE', ( #7506, #726, #27353, #27508 ) ) ;
#22590 =( NAMED_UNIT ( * ) PLANE_ANGLE_UNIT ( ) SI_UNIT ( $, .RADIAN. ) );
#22591 = ORIENTED_EDGE ( 'NONE', *, *, #14915, .T. ) ;
#22592 = CIRCLE ( 'NONE', #20356, 30.00000000000000000 ) ;
#22593 = ADVANCED_FACE ( 'NONE', ( #17400 ), #12968, .F. ) ;
#22594 = VECTOR ( 'NONE', #18684, 1000.000000000000000 ) ;
#22595 = DIRECTION ( 'NONE',  ( -0.000000000000000000, -0.000000000000000000, -1.000000000000000000 ) ) ;
#22596 = DIRECTION ( 'NONE',  ( -0.000000000000000000, 0.000000000000000000, 1.000000000000000000 ) ) ;
#22597 = ORIENTED_EDGE ( 'NONE', *, *, #22962, .F. ) ;
#22598 = ORIENTED_EDGE ( 'NONE', *, *, #2429, .F. ) ;
#22599 = LINE ( 'NONE', #9669, #9031 ) ;
#22600 = CIRCLE ( 'NONE', #8386, 5.999999999999977796 ) ;
#22601 = PLANE ( 'NONE',  #16683 ) ;
#22602 = DIRECTION ( 'NONE',  ( 0.000000000000000000, 0.000000000000000000, -1.000000000000000000 ) ) ;
#22603 = ORIENTED_EDGE ( 'NONE', *, *, #10266, .F. ) ;
#22604 = CARTESIAN_POINT ( 'NONE',  ( 158.0000000000012506, 88.08262460212675649, -45.00000000000000000 ) ) ;
#22605 = ORIENTED_EDGE ( 'NONE', *, *, #24300, .T. ) ;
#22606 = CARTESIAN_POINT ( 'NONE',  ( 2.114710523095539167E-14, -160.0000000000002274, -110.0000000000000284 ) ) ;
#22607 = EDGE_CURVE ( 'NONE', #7085, #17566, #8781, .T. ) ;
#22608 = LINE ( 'NONE', #14002, #21823 ) ;
#22609 = VECTOR ( 'NONE', #20089, 1000.000000000000000 ) ;
#22610 = DIRECTION ( 'NONE',  ( 0.8660254037844432595, 0.4999999999999918954, 0.000000000000000000 ) ) ;
#22611 = CARTESIAN_POINT ( 'NONE',  ( -23.11731384102234443, 129.3701763555853859, -16.91551946832288422 ) ) ;
#22612 = DIRECTION ( 'NONE',  ( -0.000000000000000000, 1.000000000000000000, -1.387778780781445429E-16 ) ) ;
#22613 = AXIS2_PLACEMENT_3D ( 'NONE', #2983, #12051, #3115 ) ;
#22614 = CARTESIAN_POINT ( 'NONE',  ( 144.9999999999998863, 220.0000000000000284, -119.9999999999999858 ) ) ;
#22615 = DIRECTION ( 'NONE',  ( 1.000000000000000000, 0.000000000000000000, 0.000000000000000000 ) ) ;
#22616 = ORIENTED_EDGE ( 'NONE', *, *, #26222, .F. ) ;
#22617 = AXIS2_PLACEMENT_3D ( 'NONE', #27134, #4869, #7470 ) ;
#22618 = EDGE_CURVE ( 'NONE', #9931, #17958, #22660, .T. ) ;
#22619 = DIRECTION ( 'NONE',  ( 0.4528218681373921140, 0.8916010070298049373, -0.000000000000000000 ) ) ;
#22620 = DIRECTION ( 'NONE',  ( -0.000000000000000000, 1.000000000000000000, -1.387778780781445429E-16 ) ) ;
#22622 = FACE_OUTER_BOUND ( 'NONE', #18285, .T. ) ;
#22621 = CIRCLE ( 'NONE', #23989, 41.00000000000000000 ) ;
#22623 = DIRECTION ( 'NONE',  ( 0.000000000000000000, 0.000000000000000000, -1.000000000000000000 ) ) ;
#22624 = EDGE_LOOP ( 'NONE', ( #18327, #9260, #14094, #8249 ) ) ;
#22625 = CARTESIAN_POINT ( 'NONE',  ( -260.0000000000001137, -165.0000000000001137, -59.99999999999986500 ) ) ;
#22626 = AXIS2_PLACEMENT_3D ( 'NONE', #1524, #14751, #10575 ) ;
#22627 = ORIENTED_EDGE ( 'NONE', *, *, #9227, .F. ) ;
#22628 = FACE_OUTER_BOUND ( 'NONE', #6006, .T. ) ;
#22629 = CARTESIAN_POINT ( 'NONE',  ( -235.5935699371920293, 67.74125567661748448, -5.863186529791158286 ) ) ;
#22630 = CARTESIAN_POINT ( 'NONE',  ( 139.5196418751131091, 249.6589030830498075, -148.9655004847909936 ) ) ;
#22631 = ORIENTED_EDGE ( 'NONE', *, *, #20262, .F. ) ;
#22632 = CARTESIAN_POINT ( 'NONE',  ( 134.9999999999998863, 250.0000000000000568, -151.0000000000000284 ) ) ;
#22633 = EDGE_CURVE ( 'NONE', #13806, #20506, #6762, .T. ) ;
#22634 = ORIENTED_EDGE ( 'NONE', *, *, #11680, .F. ) ;
#22635 = EDGE_CURVE ( 'NONE', #6741, #17075, #22061, .T. ) ;
#22636 = DIRECTION ( 'NONE',  ( 0.000000000000000000, 1.000000000000000000, -1.224646799147353207E-16 ) ) ;
#22637 = ORIENTED_EDGE ( 'NONE', *, *, #1533, .T. ) ;
#22638 = EDGE_CURVE ( 'NONE', #26868, #2799, #26730, .T. ) ;
#22639 = CARTESIAN_POINT ( 'NONE',  ( -275.9362193061379003, -170.0000000000001137, -102.1458326826622027 ) ) ;
#22640 = ORIENTED_EDGE ( 'NONE', *, *, #20182, .F. ) ;
#22641 = AXIS2_PLACEMENT_3D ( 'NONE', #12544, #21567, #1323 ) ;
#22642 = ORIENTED_EDGE ( 'NONE', *, *, #5592, .T. ) ;
#22643 = DIRECTION ( 'NONE',  ( -0.8916010070299070778, -0.4528218681371909971, 0.000000000000000000 ) ) ;
#22644 = ORIENTED_EDGE ( 'NONE', *, *, #11212, .T. ) ;
#22645 = AXIS2_PLACEMENT_3D ( 'NONE', #25605, #21440, #10392 ) ;
#22646 = ORIENTED_EDGE ( 'NONE', *, *, #21508, .T. ) ;
#22647 = ORIENTED_EDGE ( 'NONE', *, *, #19275, .F. ) ;
#22648 = DIRECTION ( 'NONE',  ( 0.4528218681372110921, -0.8916010070298969747, 0.000000000000000000 ) ) ;
#22649 = DIRECTION ( 'NONE',  ( -0.000000000000000000, -0.000000000000000000, -1.000000000000000000 ) ) ;
#22650 = DIRECTION ( 'NONE',  ( 0.000000000000000000, -1.000000000000000000, 0.000000000000000000 ) ) ;
#22651 = DIRECTION ( 'NONE',  ( 0.000000000000000000, -1.000000000000000000, 0.000000000000000000 ) ) ;
#22652 = PLANE ( 'NONE',  #20450 ) ;
#22653 = DIRECTION ( 'NONE',  ( 0.4528218681383106015, 0.8916010070293384215, -0.000000000000000000 ) ) ;
#22654 = FACE_OUTER_BOUND ( 'NONE', #2831, .T. ) ;
#22655 = CARTESIAN_POINT ( 'NONE',  ( 158.0000000000010232, 108.1456246621830957, 45.00000000000000000 ) ) ;
#22656 = CARTESIAN_POINT ( 'NONE',  ( -276.0548825800837562, -164.9999999997509121, 107.4689643235781489 ) ) ;
#22657 = CARTESIAN_POINT ( 'NONE',  ( 157.9999999999996874, 268.6496251426330559, 45.00000000000000000 ) ) ;
#22658 = FACE_OUTER_BOUND ( 'NONE', #17850, .T. ) ;
#22659 = ORIENTED_EDGE ( 'NONE', *, *, #149, .F. ) ;
#22660 = CIRCLE ( 'NONE', #18064, 27.00000000000002487 ) ;
#22661 = EDGE_CURVE ( 'NONE', #23530, #3711, #15406, .T. ) ;
#22662 = EDGE_CURVE ( 'NONE', #2950, #28150, #24583, .T. ) ;
#22663 = AXIS2_PLACEMENT_3D ( 'NONE', #764, #1038, #27180 ) ;
#22664 = PLANE ( 'NONE',  #23393 ) ;
#22665 = PLANE ( 'NONE',  #1138 ) ;
#22666 = DIRECTION ( 'NONE',  ( 1.000000000000000000, 1.927605262034834208E-15, 0.000000000000000000 ) ) ;
#22667 = AXIS2_PLACEMENT_3D ( 'NONE', #10991, #26625, #24335 ) ;
#22668 = EDGE_LOOP ( 'NONE', ( #19540, #24859, #18256, #21170 ) ) ;
#22669 = CARTESIAN_POINT ( 'NONE',  ( 158.0000000000016769, 47.95662448201407102, 45.00000000000000000 ) ) ;
#22670 = ORIENTED_EDGE ( 'NONE', *, *, #18993, .F. ) ;
#22671 = EDGE_CURVE ( 'NONE', #18983, #5384, #11187, .T. ) ;
#22672 = CARTESIAN_POINT ( 'NONE',  ( 158.0000000000000853, 196.4291249324366504, 45.00000000000000000 ) ) ;
#22673 = ORIENTED_EDGE ( 'NONE', *, *, #27717, .T. ) ;
#22674 = ADVANCED_FACE ( 'NONE', ( #12087 ), #7627, .F. ) ;
#22675 = ORIENTED_EDGE ( 'NONE', *, *, #24701, .F. ) ;
#22676 = ORIENTED_EDGE ( 'NONE', *, *, #4979, .F. ) ;
#22677 = VERTEX_POINT ( 'NONE', #26880 ) ;
#22678 = CARTESIAN_POINT ( 'NONE',  ( 157.9999999999996874, 266.1417501351260171, 45.00000000000000000 ) ) ;
#22679 = VECTOR ( 'NONE', #22464, 1000.000000000000000 ) ;
#22680 = DIRECTION ( 'NONE',  ( -0.000000000000000000, -0.000000000000000000, -1.000000000000000000 ) ) ;
#22681 = DIRECTION ( 'NONE',  ( -0.000000000000000000, -0.000000000000000000, -1.000000000000000000 ) ) ;
#22682 = CARTESIAN_POINT ( 'NONE',  ( -67.66675424875249689, 133.9296644792104871, -15.61820326278706972 ) ) ;
#22683 = VECTOR ( 'NONE', #22623, 1000.000000000000000 ) ;
#22684 = CARTESIAN_POINT ( 'NONE',  ( -200.0000000000000284, -91.18033988749901653, 0.000000000000000000 ) ) ;
#22685 = CARTESIAN_POINT ( 'NONE',  ( 119.4436508138959567, 203.0294372515225518, 45.00000000000000000 ) ) ;
#22686 = CARTESIAN_POINT ( 'NONE',  ( 367.4999999999996021, 44.41075299063183479, 100.0000000000000284 ) ) ;
#22687 = CARTESIAN_POINT ( 'NONE',  ( 157.4999999999998579, 223.7618125112605298, 45.00000000000000000 ) ) ;
#22688 = DIRECTION ( 'NONE',  ( 0.000000000000000000, 0.000000000000000000, -1.000000000000000000 ) ) ;
#22689 = PLANE ( 'NONE',  #21325 ) ;
#22690 = CARTESIAN_POINT ( 'NONE',  ( 157.4999999999998579, 110.9074371734436255, -45.00000000000000000 ) ) ;
#22691 = DIRECTION ( 'NONE',  ( 0.000000000000000000, 0.000000000000000000, -1.000000000000000000 ) ) ;
#22692 = CARTESIAN_POINT ( 'NONE',  ( 104.1118574119297762, 122.0584436052485700, 84.84374999969743669 ) ) ;
#22693 = EDGE_CURVE ( 'NONE', #18911, #24310, #24867, .T. ) ;
#22694 = LINE ( 'NONE', #11925, #10068 ) ;
#22695 = CARTESIAN_POINT ( 'NONE',  ( -181.4803588069671036, 108.8061799861145431, 31.29209452200661801 ) ) ;
#22696 = DIRECTION ( 'NONE',  ( -0.8916010070296531698, -0.4528218681376911525, 0.000000000000000000 ) ) ;
#22698 = ORIENTED_EDGE ( 'NONE', *, *, #16955, .F. ) ;
#22697 = EDGE_LOOP ( 'NONE', ( #820, #16663, #294, #18637 ) ) ;
#22699 = AXIS2_PLACEMENT_3D ( 'NONE', #5640, #18576, #772 ) ;
#22700 = CARTESIAN_POINT ( 'NONE',  ( -207.6601984805002132, 89.35148749558611314, -27.03156250143107897 ) ) ;
#22701 = FACE_OUTER_BOUND ( 'NONE', #21450, .T. ) ;
#22702 = EDGE_LOOP ( 'NONE', ( #2223, #26314, #6902, #17967 ) ) ;
#22703 = CIRCLE ( 'NONE', #16288, 5.999999999999977796 ) ;
#22704 = ORIENTED_EDGE ( 'NONE', *, *, #25436, .F. ) ;
#22705 = EDGE_CURVE ( 'NONE', #6158, #12778, #18541, .T. ) ;
#22706 = PLANE ( 'NONE',  #7901 ) ;
#22707 = EDGE_CURVE ( 'NONE', #8565, #12700, #20409, .T. ) ;
#22708 = CARTESIAN_POINT ( 'NONE',  ( 0.000000000000000000, 330.0000000000000000, -100.0000000000000142 ) ) ;
#22709 = VERTEX_POINT ( 'NONE', #1005 ) ;
#22710 = EDGE_LOOP ( 'NONE', ( #11659, #3098, #12780, #4018 ) ) ;
#22711 = CARTESIAN_POINT ( 'NONE',  ( 109.9999999999999005, 240.0000000000000284, -45.00000000000000000 ) ) ;
#22712 = CARTESIAN_POINT ( 'NONE',  ( -68.57415822541635464, 75.97823757117562593, 95.00000000000000000 ) ) ;
#22713 = CARTESIAN_POINT ( 'NONE',  ( -25.39999999999996305, 0.000000000000000000, 0.000000000000000000 ) ) ;
#22714 = VECTOR ( 'NONE', #25987, 1000.000000000000000 ) ;
#22715 = CARTESIAN_POINT ( 'NONE',  ( 157.9999999999998295, 231.0315000300280417, -45.00000000000000000 ) ) ;
#22716 = EDGE_CURVE ( 'NONE', #21766, #6126, #7204, .T. ) ;
#22717 = EDGE_CURVE ( 'NONE', #6126, #3644, #20267, .T. ) ;
#22718 = CARTESIAN_POINT ( 'NONE',  ( 209.9999999999999432, 0.000000000000000000, -99.99999999999995737 ) ) ;
#22719 = AXIS2_PLACEMENT_3D ( 'NONE', #4237, #28349, #8697 ) ;
#22720 = CARTESIAN_POINT ( 'NONE',  ( -160.0000000000000284, 109.9999999999999432, 70.00000000000001421 ) ) ;
#22721 = CARTESIAN_POINT ( 'NONE',  ( -205.1716483941798401, 60.34345434848681577, -21.58965668827011442 ) ) ;
#22722 = CARTESIAN_POINT ( 'NONE',  ( 3.469446951953618133E-15, -50.00000000000004263, 98.28427124746191623 ) ) ;
#22723 = EDGE_CURVE ( 'NONE', #970, #2675, #739, .T. ) ;
#22724 = CARTESIAN_POINT ( 'NONE',  ( 157.4999999999998295, 218.7460624962465090, -45.00000000000000000 ) ) ;
#22725 = CARTESIAN_POINT ( 'NONE',  ( 157.4999999999998579, 161.0649373235845019, -45.00000000000000000 ) ) ;
#22726 = CARTESIAN_POINT ( 'NONE',  ( 158.0000000000001990, 188.3976249024084666, -45.00000000000000000 ) ) ;
#22727 = ORIENTED_EDGE ( 'NONE', *, *, #20538, .F. ) ;
#22728 = CARTESIAN_POINT ( 'NONE',  ( 65.00000000000000000, -170.0000000000000568, 70.00000000000001421 ) ) ;
#22729 = CARTESIAN_POINT ( 'NONE',  ( -237.0233935005625767, 68.72940251376630272, 14.95240471282495598 ) ) ;
#22730 = DIRECTION ( 'NONE',  ( -0.000000000000000000, -0.000000000000000000, -1.000000000000000000 ) ) ;
#22731 = EDGE_LOOP ( 'NONE', ( #13233, #8832, #6934, #10849 ) ) ;
#22732 = VECTOR ( 'NONE', #14553, 1000.000000000000000 ) ;
#22733 = ORIENTED_EDGE ( 'NONE', *, *, #18084, .F. ) ;
#22734 = VECTOR ( 'NONE', #10015, 1000.000000000000114 ) ;
#22735 = LINE ( 'NONE', #27033, #1461 ) ;
#22736 = DIRECTION ( 'NONE',  ( 0.000000000000000000, 0.000000000000000000, 1.000000000000000000 ) ) ;
#22737 = ORIENTED_EDGE ( 'NONE', *, *, #10490, .F. ) ;
#22738 = AXIS2_PLACEMENT_3D ( 'NONE', #9326, #9612, #18232 ) ;
#22739 = AXIS2_PLACEMENT_3D ( 'NONE', #27856, #8197, #16961 ) ;
#22740 = ORIENTED_EDGE ( 'NONE', *, *, #24461, .F. ) ;
#22741 = DIRECTION ( 'NONE',  ( 0.000000000000000000, 0.000000000000000000, 1.000000000000000000 ) ) ;
#22742 = FACE_OUTER_BOUND ( 'NONE', #915, .T. ) ;
#22743 = CARTESIAN_POINT ( 'NONE',  ( 157.4999999999998579, 48.21056198576756202, 45.00000000000000000 ) ) ;
#22744 = VERTEX_POINT ( 'NONE', #18263 ) ;
#22745 = PLANE ( 'NONE',  #18337 ) ;
#22746 = ORIENTED_EDGE ( 'NONE', *, *, #24082, .T. ) ;
#22747 = DIRECTION ( 'NONE',  ( 0.000000000000000000, 0.000000000000000000, -1.000000000000000000 ) ) ;
#22748 = DIRECTION ( 'NONE',  ( 4.540956701092242152E-16, 1.000000000000000000, 0.000000000000000000 ) ) ;
#22749 = AXIS2_PLACEMENT_3D ( 'NONE', #25111, #16088, #5149 ) ;
#22750 = CARTESIAN_POINT ( 'NONE',  ( -216.4421519707229606, 141.6000904446840991, 13.00000000000000000 ) ) ;
#22751 = CARTESIAN_POINT ( 'NONE',  ( -18.04820575590032661, 129.9789000731339570, -16.68755046163289535 ) ) ;
#22752 = VECTOR ( 'NONE', #16333, 1000.000000000000000 ) ;
#22753 = CARTESIAN_POINT ( 'NONE',  ( 372.9108539694884144, 19.41075299063184900, 87.99671038392668265 ) ) ;
#22755 = EDGE_CURVE ( 'NONE', #3702, #3368, #13028, .T. ) ;
#22754 = AXIS2_PLACEMENT_3D ( 'NONE', #4101, #21630, #11006 ) ;
#22756 = EDGE_CURVE ( 'NONE', #8677, #11330, #599, .T. ) ;
#22757 = CARTESIAN_POINT ( 'NONE',  ( -274.7557459110829541, -165.0000000000001137, -86.12025961983451339 ) ) ;
#22758 = DIRECTION ( 'NONE',  ( -1.000000000000000000, 6.752478448789676648E-18, 0.000000000000000000 ) ) ;
#22759 = ORIENTED_EDGE ( 'NONE', *, *, #21419, .T. ) ;
#22760 = FACE_BOUND ( 'NONE', #895, .T. ) ;
#22761 = EDGE_CURVE ( 'NONE', #3887, #22709, #1151, .T. ) ;
#22762 = VECTOR ( 'NONE', #22250, 1000.000000000000114 ) ;
#22763 = CARTESIAN_POINT ( 'NONE',  ( -17.24491960465745777, 29.64876300893806516, 95.00000000000000000 ) ) ;
#22764 = LINE ( 'NONE', #7809, #5218 ) ;
#22765 = EDGE_LOOP ( 'NONE', ( #26677, #7036, #19299, #684, #25452, #2833 ) ) ;
#22766 = DIRECTION ( 'NONE',  ( 8.659560562354934091E-17, 0.7071067811865474617, -0.7071067811865476838 ) ) ;
#22767 = ORIENTED_EDGE ( 'NONE', *, *, #25944, .T. ) ;
#22768 = FACE_OUTER_BOUND ( 'NONE', #11406, .T. ) ;
#22769 = CARTESIAN_POINT ( 'NONE',  ( 157.4999999999996589, 273.9193126614005678, -45.00000000000000000 ) ) ;
#22770 = LINE ( 'NONE', #927, #21793 ) ;
#22771 = ORIENTED_EDGE ( 'NONE', *, *, #17804, .F. ) ;
#22772 = LINE ( 'NONE', #2648, #3729 ) ;
#22773 = CARTESIAN_POINT ( 'NONE',  ( 22.58950924271104910, 154.2349915562422780, 15.00000000000000000 ) ) ;
#22774 = EDGE_LOOP ( 'NONE', ( #15757, #18468, #4027, #13111 ) ) ;
#22775 = CARTESIAN_POINT ( 'NONE',  ( -52.81561984911300556, 131.8400808202090957, 16.12034709971533886 ) ) ;
#22776 = CARTESIAN_POINT ( 'NONE',  ( 98.49257838773085894, 241.8754478897298839, 12.06630627437291992 ) ) ;
#22777 = ORIENTED_EDGE ( 'NONE', *, *, #7156, .F. ) ;
#22778 = VECTOR ( 'NONE', #24081, 1000.000000000000227 ) ;
#22779 = ORIENTED_EDGE ( 'NONE', *, *, #3351, .F. ) ;
#22780 = DIRECTION ( 'NONE',  ( 0.5000000000000039968, 0.8660254037844362651, 0.000000000000000000 ) ) ;
#22781 = ORIENTED_EDGE ( 'NONE', *, *, #11239, .T. ) ;
#22782 = ORIENTED_EDGE ( 'NONE', *, *, #21351, .F. ) ;
#22783 =( BOUNDED_CURVE ( )  B_SPLINE_CURVE ( 2, ( #25045, #16564, #18711 ),
 .UNSPECIFIED., .F., .F. ) 
 B_SPLINE_CURVE_WITH_KNOTS ( ( 3, 3 ),
 ( 0.000000000000000000, 1.000000000000000000 ),
 .UNSPECIFIED. ) 
 CURVE ( )  GEOMETRIC_REPRESENTATION_ITEM ( )  RATIONAL_B_SPLINE_CURVE ( ( 1.000000000000000000, 0.7071067811865484609, 1.000000000000000000 ) ) 
 REPRESENTATION_ITEM ( '' )  );
#22784 = ORIENTED_EDGE ( 'NONE', *, *, #24127, .F. ) ;
#22785 = PLANE ( 'NONE',  #27171 ) ;
#22786 = DIRECTION ( 'NONE',  ( 0.000000000000000000, 0.000000000000000000, 1.000000000000000000 ) ) ;
#22787 = EDGE_CURVE ( 'NONE', #24673, #17712, #26176, .T. ) ;
#22788 = CARTESIAN_POINT ( 'NONE',  ( 158.0000000000017053, 43.44874947450702507, 45.00000000000000000 ) ) ;
#22789 = EDGE_CURVE ( 'NONE', #4657, #3701, #1290, .T. ) ;
#22790 = EDGE_CURVE ( 'NONE', #4583, #23257, #17082, .T. ) ;
#22791 = CARTESIAN_POINT ( 'NONE',  ( 82.68942924499074820, 110.0997128786250840, -70.07812500014861712 ) ) ;
#22792 = DIRECTION ( 'NONE',  ( 0.000000000000000000, 0.000000000000000000, -1.000000000000000000 ) ) ;
#22793 = DIRECTION ( 'NONE',  ( -0.000000000000000000, 0.000000000000000000, 1.000000000000000000 ) ) ;
#22794 = EDGE_CURVE ( 'NONE', #12610, #27327, #27559, .T. ) ;
#22795 = CARTESIAN_POINT ( 'NONE',  ( 157.9999999999996874, 266.6496251426330559, -45.00000000000000000 ) ) ;
#22796 = FACE_OUTER_BOUND ( 'NONE', #3422, .T. ) ;
#22797 = DIRECTION ( 'NONE',  ( -1.000000000000000000, 0.000000000000000000, 0.000000000000000000 ) ) ;
#22798 = DIRECTION ( 'NONE',  ( -0.000000000000000000, -0.000000000000000000, -1.000000000000000000 ) ) ;
#22799 = CARTESIAN_POINT ( 'NONE',  ( 114.6895484223570918, 210.2681915721689450, -98.48649515991441206 ) ) ;
#22800 = AXIS2_PLACEMENT_3D ( 'NONE', #13890, #2657, #7410 ) ;
#22801 = ORIENTED_EDGE ( 'NONE', *, *, #7625, .T. ) ;
#22802 = CARTESIAN_POINT ( 'NONE',  ( 0.9552291512637759441, -1.250000000000000444, 7.454565938624107879 ) ) ;
#22803 = PLANE ( 'NONE',  #12621 ) ;
#22804 = PLANE ( 'NONE',  #12031 ) ;
#22805 = B_SPLINE_CURVE_WITH_KNOTS ( 'NONE', 3,
 ( #20661, #846, #5151, #2849, #9615, #27126, #16090, #2991, #24694, #7459, #15945, #18650, #11783, #16230, #24979, #7171, #14076, #5002 ),
 .UNSPECIFIED., .F., .F.,
 ( 4, 2, 2, 2, 2, 2, 2, 2, 4 ),
 ( 0.000000000000000000, 0.1250000000000000000, 0.2500000000000000000, 0.3750000000000000000, 0.5000000000000000000, 0.6250000000000000000, 0.7500000000000000000, 0.8750000000000000000, 1.000000000000000000 ),
 .UNSPECIFIED. ) ;
#22806 = EDGE_LOOP ( 'NONE', ( #11546, #3849, #19522, #4286 ) ) ;
#22807 = CYLINDRICAL_SURFACE ( 'NONE', #9785, 49.99999999999998579 ) ;
#22808 = ORIENTED_EDGE ( 'NONE', *, *, #124, .T. ) ;
#22809 = CARTESIAN_POINT ( 'NONE',  ( 157.4999999999995168, 208.7145624662163925, 45.00000000000000000 ) ) ;
#22810 = EDGE_LOOP ( 'NONE', ( #2207, #20991 ) ) ;
#22811 = ORIENTED_EDGE ( 'NONE', *, *, #2140, .F. ) ;
#22812 = ORIENTED_EDGE ( 'NONE', *, *, #2225, .T. ) ;
#22813 = EDGE_LOOP ( 'NONE', ( #23645, #15296, #20880, #2170 ) ) ;
#22814 = CARTESIAN_POINT ( 'NONE',  ( 158.0000000000017053, 45.44874947450702507, -45.00000000000000000 ) ) ;
#22815 = VECTOR ( 'NONE', #16419, 1000.000000000000000 ) ;
#22816 = LINE ( 'NONE', #1115, #6308 ) ;
#22817 = CARTESIAN_POINT ( 'NONE',  ( -210.0000000000000568, -152.0000000000000284, -105.0000000000000284 ) ) ;
#22818 = ADVANCED_FACE ( 'NONE', ( #14516 ), #7964, .F. ) ;
#22819 = EDGE_CURVE ( 'NONE', #10398, #548, #23408, .T. ) ;
#22820 = CARTESIAN_POINT ( 'NONE',  ( -52.45095902829482526, 133.2634102098851372, -14.19419100766092257 ) ) ;
#22821 = CARTESIAN_POINT ( 'NONE',  ( 0.000000000000000000, 1.249999999999999556, 8.000000000000000000 ) ) ;
#22822 = ADVANCED_FACE ( 'NONE', ( #21251 ), #3437, .T. ) ;
#22823 = CARTESIAN_POINT ( 'NONE',  ( -207.5699030661693030, 75.55056756148773900, 43.24289214104831558 ) ) ;
#22824 = DIRECTION ( 'NONE',  ( 0.000000000000000000, 1.272130549049657961E-16, -1.000000000000000000 ) ) ;
#22825 = CARTESIAN_POINT ( 'NONE',  ( -52.44999544250409684, 133.2632066869771563, -14.19424921271702011 ) ) ;
#22826 = ADVANCED_FACE ( 'NONE', ( #10480 ), #20969, .F. ) ;
#22827 = CARTESIAN_POINT ( 'NONE',  ( 167.4999999999996589, -5.589247009368156327, 74.99999999999995737 ) ) ;
#22828 = CARTESIAN_POINT ( 'NONE',  ( -227.0596193454513525, 90.08420170043139308, -13.60108752251566244 ) ) ;
#22829 = PLANE ( 'NONE',  #23923 ) ;
#22830 = CARTESIAN_POINT ( 'NONE',  ( 167.4999999999996589, 494.4107529906318632, 74.99999999999995737 ) ) ;
#22831 = CARTESIAN_POINT ( 'NONE',  ( -34.12965183067004205, -18.01420295945611727, 100.0000000000000000 ) ) ;
#22832 = LINE ( 'NONE', #5301, #9146 ) ;
#22833 = CARTESIAN_POINT ( 'NONE',  ( 96.76194576697405125, 83.89264379418708018, -100.0000000000000284 ) ) ;
#22834 = DIRECTION ( 'NONE',  ( -1.000000000000000000, 0.000000000000000000, 0.000000000000000000 ) ) ;
#22836 = ORIENTED_EDGE ( 'NONE', *, *, #946, .F. ) ;
#22835 = EDGE_LOOP ( 'NONE', ( #24960, #12154, #13346 ) ) ;
#22837 = VECTOR ( 'NONE', #15797, 1000.000000000000227 ) ;
#22838 = CARTESIAN_POINT ( 'NONE',  ( -236.8667578982872044, 138.8517089611673043, 5.000000000000002665 ) ) ;
#22839 = EDGE_LOOP ( 'NONE', ( #22413, #15646, #3453, #12845 ) ) ;
#22840 = ORIENTED_EDGE ( 'NONE', *, *, #3191, .T. ) ;
#22841 = CARTESIAN_POINT ( 'NONE',  ( -261.1919288306253293, -171.9377729149742038, -94.99999999999987210 ) ) ;
#22842 = ORIENTED_EDGE ( 'NONE', *, *, #20583, .F. ) ;
#22843 = ORIENTED_EDGE ( 'NONE', *, *, #27306, .T. ) ;
#22844 = LINE ( 'NONE', #5451, #25240 ) ;
#22845 = CARTESIAN_POINT ( 'NONE',  ( 157.4999999999998295, 226.2696875187675118, 45.00000000000000000 ) ) ;
#22846 = AXIS2_PLACEMENT_3D ( 'NONE', #19672, #24134, #13221 ) ;
#22847 = EDGE_CURVE ( 'NONE', #7652, #10728, #12369, .T. ) ;
#22848 = CONICAL_SURFACE ( 'NONE', #15060, 6.025000000000002132, 0.7853981633974482790 ) ;
#22849 = CYLINDRICAL_SURFACE ( 'NONE', #19236, 5.999999999999991118 ) ;
#22850 = B_SPLINE_CURVE_WITH_KNOTS ( 'NONE', 3,
 ( #19575, #15556, #24305, #28311, #8659, #6496, #24033, #8793, #17552, #26315, #4611, #6640, #15419, #13400 ),
 .UNSPECIFIED., .F., .F.,
 ( 4, 2, 2, 2, 2, 2, 4 ),
 ( 0.000000000000000000, 0.001215459952587881953, 0.001823189928881842770, 0.002430919905175803804, 0.003038649881469764405, 0.003646379857763725439, 0.004861839810351617150 ),
 .UNSPECIFIED. ) ;
#22851 = DIRECTION ( 'NONE',  ( 0.5150380749100565980, 0.000000000000000000, -0.8571673007021108903 ) ) ;
#22852 = LINE ( 'NONE', #9788, #19488 ) ;
#22853 = DIRECTION ( 'NONE',  ( -1.000000000000000000, -1.233581138472397295E-15, 0.000000000000000000 ) ) ;
#22854 = CARTESIAN_POINT ( 'NONE',  ( -219.7112380651048227, 60.27397245185819230, -23.81555219816717894 ) ) ;
#22855 = ADVANCED_FACE ( 'NONE', ( #16945 ), #25699, .T. ) ;
#22856 = CARTESIAN_POINT ( 'NONE',  ( 157.9999999999998010, 234.0472500450420341, 45.00000000000000000 ) ) ;
#22857 = DIRECTION ( 'NONE',  ( 8.673617379884037937E-17, -1.000000000000000000, 0.000000000000000000 ) ) ;
#22858 = CARTESIAN_POINT ( 'NONE',  ( 153.4775906502256930, 212.3463313526982859, 45.00000000000000000 ) ) ;
#22859 = PLANE ( 'NONE',  #9842 ) ;
#22860 = ORIENTED_EDGE ( 'NONE', *, *, #25330, .T. ) ;
#22861 = LINE ( 'NONE', #24596, #5479 ) ;
#22862 = VECTOR ( 'NONE', #5401, 999.9999999999998863 ) ;
#22863 = CARTESIAN_POINT ( 'NONE',  ( -229.4479296852373409, 74.49644851802749201, 16.38316105113803545 ) ) ;
#22864 = AXIS2_PLACEMENT_3D ( 'NONE', #6946, #26472, #23771 ) ;
#22865 = DIRECTION ( 'NONE',  ( -0.8916010070295614653, 0.4528218681378716193, 0.000000000000000000 ) ) ;
#22866 = ORIENTED_EDGE ( 'NONE', *, *, #6941, .F. ) ;
#22867 = CARTESIAN_POINT ( 'NONE',  ( -175.0000000000000000, -114.0000000000001563, 70.00000000000001421 ) ) ;
#22868 = ORIENTED_EDGE ( 'NONE', *, *, #16649, .T. ) ;
#22869 = EDGE_CURVE ( 'NONE', #17461, #4617, #12789, .T. ) ;
#22870 = CARTESIAN_POINT ( 'NONE',  ( 104.1118574116920428, 122.0584436054522257, 100.0000000000000142 ) ) ;
#22871 = CARTESIAN_POINT ( 'NONE',  ( 122.6339745962156229, 200.5814157129576074, 45.00000000000000000 ) ) ;
#22872 = ORIENTED_EDGE ( 'NONE', *, *, #27628, .F. ) ;
#22873 = ORIENTED_EDGE ( 'NONE', *, *, #10889, .F. ) ;
#22874 = LINE ( 'NONE', #20573, #17303 ) ;
#22875 = ADVANCED_FACE ( 'NONE', ( #21395 ), #10059, .F. ) ;
#22876 = CARTESIAN_POINT ( 'NONE',  ( 157.4999999999998579, 125.9546872184859012, -45.00000000000000000 ) ) ;
#22877 = LINE ( 'NONE', #13996, #3151 ) ;
#22878 = ORIENTED_EDGE ( 'NONE', *, *, #23525, .F. ) ;
#22879 = CARTESIAN_POINT ( 'NONE',  ( 9.999999999999738876, -50.00000000000004263, 80.00000000000001421 ) ) ;
#22880 = ORIENTED_EDGE ( 'NONE', *, *, #18746, .F. ) ;
#22881 = CARTESIAN_POINT ( 'NONE',  ( 134.9999999999998579, 330.0000000000000000, -84.99999999999995737 ) ) ;
#22882 = AXIS2_PLACEMENT_3D ( 'NONE', #24774, #9548, #5081 ) ;
#22883 = CIRCLE ( 'NONE', #3590, 5.000000000000004441 ) ;
#22884 = CARTESIAN_POINT ( 'NONE',  ( -160.0000000000000568, 139.9999999999999716, 15.00000000000000000 ) ) ;
#22885 = CARTESIAN_POINT ( 'NONE',  ( 2.399999999999999911, 1.249999999999999556, 8.000000000000000000 ) ) ;
#22886 = CYLINDRICAL_SURFACE ( 'NONE', #10839, 10.00000000000000888 ) ;
#22887 = LINE ( 'NONE', #27323, #20987 ) ;
#22888 = VECTOR ( 'NONE', #28297, 1000.000000000000114 ) ;
#22889 = EDGE_CURVE ( 'NONE', #19795, #26495, #10200, .T. ) ;
#22890 = CARTESIAN_POINT ( 'NONE',  ( 217.4999999999996305, 83.06687458711267880, -42.86484227207692754 ) ) ;
#22891 = DIRECTION ( 'NONE',  ( -0.000000000000000000, -0.000000000000000000, -1.000000000000000000 ) ) ;
#22892 = ORIENTED_EDGE ( 'NONE', *, *, #2904, .T. ) ;
#22893 = EDGE_CURVE ( 'NONE', #1534, #4885, #27420, .T. ) ;
#22894 = DIRECTION ( 'NONE',  ( 1.000000000000000000, 1.321694076934710155E-16, 0.000000000000000000 ) ) ;
#22895 = DIRECTION ( 'NONE',  ( 0.7071067811865475727, -0.7071067811865475727, 0.000000000000000000 ) ) ;
#22896 = DIRECTION ( 'NONE',  ( -0.8916010070293384215, 0.4528218681383106015, 0.000000000000000000 ) ) ;
#22897 = ORIENTED_EDGE ( 'NONE', *, *, #13406, .T. ) ;
#22898 = DIRECTION ( 'NONE',  ( -0.8916010070293547418, -0.4528218681382785715, 0.000000000000000000 ) ) ;
#22899 = ORIENTED_EDGE ( 'NONE', *, *, #5299, .T. ) ;
#22900 = VECTOR ( 'NONE', #20882, 1000.000000000000114 ) ;
#22901 = CYLINDRICAL_SURFACE ( 'NONE', #7943, 10.00000000000000888 ) ;
#22902 = LINE ( 'NONE', #18729, #14704 ) ;
#22903 = DIRECTION ( 'NONE',  ( 0.000000000000000000, 0.000000000000000000, -1.000000000000000000 ) ) ;
#22904 = ORIENTED_EDGE ( 'NONE', *, *, #5794, .T. ) ;
#22905 = VECTOR ( 'NONE', #27870, 1000.000000000000114 ) ;
#22906 = CARTESIAN_POINT ( 'NONE',  ( 119.4436508138957720, 236.9705627484767376, -45.00000000000000000 ) ) ;
#22907 = EDGE_LOOP ( 'NONE', ( #26902, #22063, #21411, #6160 ) ) ;
#22908 = EDGE_CURVE ( 'NONE', #21163, #25781, #17786, .T. ) ;
#22909 = VECTOR ( 'NONE', #25823, 999.9999999999998863 ) ;
#22910 = CARTESIAN_POINT ( 'NONE',  ( -82.67666394482243675, 134.7683680720327573, 15.45968317728961594 ) ) ;
#22911 = FACE_OUTER_BOUND ( 'NONE', #11908, .T. ) ;
#22912 = ORIENTED_EDGE ( 'NONE', *, *, #28284, .T. ) ;
#22913 = EDGE_CURVE ( 'NONE', #25491, #23391, #19665, .T. ) ;
#22914 = ORIENTED_EDGE ( 'NONE', *, *, #27980, .F. ) ;
#22916 = EDGE_CURVE ( 'NONE', #25350, #24989, #21958, .T. ) ;
#22915 = AXIS2_PLACEMENT_3D ( 'NONE', #15509, #24399, #24123 ) ;
#22917 = CARTESIAN_POINT ( 'NONE',  ( 410.1240808061609187, 61.15703788601284430, 393.1631314933625845 ) ) ;
#22918 = ORIENTED_EDGE ( 'NONE', *, *, #12799, .T. ) ;
#22919 = EDGE_CURVE ( 'NONE', #16524, #8650, #10906, .T. ) ;
#22920 = VERTEX_POINT ( 'NONE', #26542 ) ;
#22921 = ORIENTED_EDGE ( 'NONE', *, *, #25473, .F. ) ;
#22922 = CARTESIAN_POINT ( 'NONE',  ( 109.9999999999999005, 260.0000000000000000, 45.00000000000000000 ) ) ;
#22923 = VECTOR ( 'NONE', #857, 1000.000000000000000 ) ;
#22924 = LINE ( 'NONE', #20198, #15854 ) ;
#22925 = CARTESIAN_POINT ( 'NONE',  ( -216.4421519707229606, 141.6000904446840991, 15.00000000000000000 ) ) ;
#22926 = CARTESIAN_POINT ( 'NONE',  ( 108.2273028572353297, 129.5338070842080924, -88.59375000024363089 ) ) ;
#22927 = VECTOR ( 'NONE', #2968, 1000.000000000000000 ) ;
#22928 = DIRECTION ( 'NONE',  ( 0.000000000000000000, 0.000000000000000000, -1.000000000000000000 ) ) ;
#22929 = DIRECTION ( 'NONE',  ( -0.000000000000000000, 0.000000000000000000, -1.000000000000000000 ) ) ;
#22930 = CARTESIAN_POINT ( 'NONE',  ( 157.9999999999996874, 269.1575001501400379, 45.00000000000000000 ) ) ;
#22931 = ADVANCED_FACE ( 'NONE', ( #277 ), #2916, .F. ) ;
#22932 = LINE ( 'NONE', #3379, #9240 ) ;
#22933 = PLANE ( 'NONE',  #3610 ) ;
#22934 = DIRECTION ( 'NONE',  ( 0.3102637045530683979, -0.9506505318133506854, 0.000000000000000000 ) ) ;
#22935 = ORIENTED_EDGE ( 'NONE', *, *, #26446, .F. ) ;
#22936 = AXIS2_PLACEMENT_3D ( 'NONE', #13934, #16361, #11635 ) ;
#22937 = CARTESIAN_POINT ( 'NONE',  ( 95.84668550246941265, 240.8689031315771558, -9.670617930119313144 ) ) ;
#22938 = DIRECTION ( 'NONE',  ( 0.4528218681382754074, -0.8916010070293562961, 0.000000000000000000 ) ) ;
#22939 = LINE ( 'NONE', #1240, #2821 ) ;
#22940 = EDGE_LOOP ( 'NONE', ( #17491, #21072, #22892, #14565 ) ) ;
#22941 = TOROIDAL_SURFACE ( 'NONE', #8255, 7.108535549237485540, 0.4000000000000000222 ) ;
#22942 = LINE ( 'NONE', #20782, #11627 ) ;
#22943 = ORIENTED_EDGE ( 'NONE', *, *, #14697, .T. ) ;
#22944 = DIRECTION ( 'NONE',  ( 0.000000000000000000, 0.000000000000000000, -1.000000000000000000 ) ) ;
#22945 = VECTOR ( 'NONE', #2705, 999.9999999999998863 ) ;
#22946 = EDGE_CURVE ( 'NONE', #12922, #8771, #4710, .T. ) ;
#22947 = EDGE_LOOP ( 'NONE', ( #19406, #23232, #5279, #14854 ) ) ;
#22948 = EDGE_CURVE ( 'NONE', #22744, #4103, #19528, .T. ) ;
#22949 = AXIS2_PLACEMENT_3D ( 'NONE', #14242, #16808, #9787 ) ;
#22950 = ORIENTED_EDGE ( 'NONE', *, *, #17597, .F. ) ;
#22951 = ORIENTED_EDGE ( 'NONE', *, *, #10922, .F. ) ;
#22952 = ORIENTED_EDGE ( 'NONE', *, *, #2082, .F. ) ;
#22953 = CARTESIAN_POINT ( 'NONE',  ( -180.0000000000000284, -70.00000000000004263, 25.00000000000000000 ) ) ;
#22954 = LINE ( 'NONE', #7592, #5011 ) ;
#22955 = LINE ( 'NONE', #21075, #19380 ) ;
#22956 = CARTESIAN_POINT ( 'NONE',  ( -62.53415162963487717, 134.9206139158971780, -15.37869918857521334 ) ) ;
#22957 = LINE ( 'NONE', #24545, #16261 ) ;
#22958 = DIRECTION ( 'NONE',  ( 0.000000000000000000, 0.000000000000000000, -1.000000000000000000 ) ) ;
#22959 = LINE ( 'NONE', #24977, #21486 ) ;
#22960 = CARTESIAN_POINT ( 'NONE',  ( -158.6374707261681465, 121.2406993230886201, -20.46622289123956762 ) ) ;
#22961 = VECTOR ( 'NONE', #26506, 1000.000000000000000 ) ;
#22962 = EDGE_CURVE ( 'NONE', #9868, #548, #15372, .T. ) ;
#22963 = DIRECTION ( 'NONE',  ( -0.000000000000000000, -0.000000000000000000, -1.000000000000000000 ) ) ;
#22964 = CARTESIAN_POINT ( 'NONE',  ( -209.0082310152468779, 89.44643712831107507, -24.31564584614111268 ) ) ;
#22966 = B_SPLINE_CURVE_WITH_KNOTS ( 'NONE', 3,
 ( #6944, #15445, #2340, #24058, #11121, #4362, #203, #13152, #21892, #15729, #8964, #17723, #26469, #24328, #4638, #24478, #4785, #13573, #1919, #18163, #11985, #27325 ),
 .UNSPECIFIED., .F., .F.,
 ( 4, 2, 2, 2, 2, 2, 2, 2, 2, 2, 4 ),
 ( 0.000000000000000000, 0.004058198178794836415, 0.006087297268192255056, 0.008116396357589672830, 0.01623279271517933872, 0.02029099089397414998, 0.02434918907276896471, 0.02840738725156378292, 0.03043648634096116773, 0.03145103588565986708, 0.03246558543035856642 ),
 .UNSPECIFIED. ) ;
#22965 =( NAMED_UNIT ( * ) PLANE_ANGLE_UNIT ( ) SI_UNIT ( $, .RADIAN. ) );
#22967 = DIRECTION ( 'NONE',  ( -1.000000000000000000, 0.000000000000000000, 0.000000000000000000 ) ) ;
#22968 = CARTESIAN_POINT ( 'NONE',  ( -63.57415822541634043, 29.64876300893806516, 95.00000000000000000 ) ) ;
#22969 = VERTEX_POINT ( 'NONE', #26124 ) ;
#22970 = AXIS2_PLACEMENT_3D ( 'NONE', #21010, #1335, #8228 ) ;
#22971 = CARTESIAN_POINT ( 'NONE',  ( -41.48633590429507478, -19.07744248478647009, 99.88564445205030040 ) ) ;
#22972 = CARTESIAN_POINT ( 'NONE',  ( -196.7519430251776384, 98.10118020365993630, 32.13010062293410130 ) ) ;
#22973 = CARTESIAN_POINT ( 'NONE',  ( 158.0000000000003695, 171.3503748573662051, 45.00000000000000000 ) ) ;
#22975 = ORIENTED_EDGE ( 'NONE', *, *, #17104, .T. ) ;
#22974 = ORIENTED_EDGE ( 'NONE', *, *, #3278, .F. ) ;
#22976 = DIRECTION ( 'NONE',  ( 0.000000000000000000, 0.000000000000000000, -1.000000000000000000 ) ) ;
#22977 = ORIENTED_EDGE ( 'NONE', *, *, #21294, .T. ) ;
#22978 = ORIENTED_EDGE ( 'NONE', *, *, #7125, .T. ) ;
#22979 = EDGE_CURVE ( 'NONE', #13271, #5384, #13491, .T. ) ;
#22980 = ORIENTED_EDGE ( 'NONE', *, *, #27367, .F. ) ;
#22981 = EDGE_CURVE ( 'NONE', #2545, #6857, #11193, .T. ) ;
#22982 = VECTOR ( 'NONE', #2709, 1000.000000000000227 ) ;
#22983 = ADVANCED_FACE ( 'NONE', ( #26404 ), #13353, .F. ) ;
#22984 = ORIENTED_EDGE ( 'NONE', *, *, #18472, .F. ) ;
#22985 = VERTEX_POINT ( 'NONE', #15653 ) ;
#22986 = CARTESIAN_POINT ( 'NONE',  ( 157.6866818850739662, 8.471341669691319964, 45.00000000000000000 ) ) ;
#22987 = CARTESIAN_POINT ( 'NONE',  ( 267.4999999999996021, 194.4107529906318064, 100.0000000000000284 ) ) ;
#22988 = VECTOR ( 'NONE', #27429, 1000.000000000000000 ) ;
#22989 = LINE ( 'NONE', #2881, #1796 ) ;
#22990 = CARTESIAN_POINT ( 'NONE',  ( 98.66165036324171922, 233.9456810963309579, -21.50628274051351951 ) ) ;
#22991 = DIRECTION ( 'NONE',  ( -0.000000000000000000, -0.000000000000000000, -1.000000000000000000 ) ) ;
#22992 = LINE ( 'NONE', #20550, #15381 ) ;
#22993 = LINE ( 'NONE', #27990, #6369 ) ;
#22994 = CARTESIAN_POINT ( 'NONE',  ( -207.8780609232275651, 75.32569699198245416, -40.84837702943764981 ) ) ;
#22995 = VECTOR ( 'NONE', #24231, 1000.000000000000000 ) ;
#22996 = CARTESIAN_POINT ( 'NONE',  ( 110.1465075748078277, 203.1971239227096646, -150.6145052419835224 ) ) ;
#22997 = CARTESIAN_POINT ( 'NONE',  ( 124.3660254037845192, 199.5814157129575506, 45.00000000000000000 ) ) ;
#22998 = DIRECTION ( 'NONE',  ( 0.000000000000000000, 0.000000000000000000, -1.000000000000000000 ) ) ;
#22999 = DIRECTION ( 'NONE',  ( 0.4528218681383056610, -0.8916010070293409751, 0.000000000000000000 ) ) ;
#23000 = ORIENTED_EDGE ( 'NONE', *, *, #3251, .F. ) ;
#23001 = CARTESIAN_POINT ( 'NONE',  ( -200.0065789263009037, 95.74113499274756123, 30.18550423898969015 ) ) ;
#23002 = CIRCLE ( 'NONE', #12477, 3.532530335305414493 ) ;
#23003 = EDGE_CURVE ( 'NONE', #9740, #24079, #2269, .T. ) ;
#23004 = CARTESIAN_POINT ( 'NONE',  ( -210.0000000000000568, -280.0000000000000000, 110.0000000000000284 ) ) ;
#23005 = EDGE_LOOP ( 'NONE', ( #25038, #19557, #5367, #15007 ) ) ;
#23006 = ORIENTED_EDGE ( 'NONE', *, *, #26151, .F. ) ;
#23007 = CARTESIAN_POINT ( 'NONE',  ( 93.07270601802888166, 112.9533406971467429, 74.06249999970600584 ) ) ;
#23008 = DIRECTION ( 'NONE',  ( -0.8916010070294503320, -0.4528218681380901667, 0.000000000000000000 ) ) ;
#23009 = EDGE_CURVE ( 'NONE', #695, #20671, #13411, .T. ) ;
#23010 = EDGE_LOOP ( 'NONE', ( #4810, #12801 ) ) ;
#23011 = EDGE_LOOP ( 'NONE', ( #4652, #27939, #27895, #10859 ) ) ;
#23012 = FACE_OUTER_BOUND ( 'NONE', #13444, .T. ) ;
#23013 = ADVANCED_FACE ( 'NONE', ( #4428 ), #7548, .T. ) ;
#23014 = AXIS2_PLACEMENT_3D ( 'NONE', #20458, #22895, #781 ) ;
#23015 = DIRECTION ( 'NONE',  ( 1.000000000000000000, 0.000000000000000000, 0.000000000000000000 ) ) ;
#23016 = CARTESIAN_POINT ( 'NONE',  ( 217.4999999999996305, 258.6181251126050711, -5.999999999999991118 ) ) ;
#23017 = ORIENTED_EDGE ( 'NONE', *, *, #15411, .T. ) ;
#23018 = DIRECTION ( 'NONE',  ( 2.775557561562887407E-16, 3.668437989309015850E-32, 1.000000000000000000 ) ) ;
#23019 = ORIENTED_EDGE ( 'NONE', *, *, #27961, .T. ) ;
#23020 = VECTOR ( 'NONE', #11397, 1000.000000000000000 ) ;
#23021 = VECTOR ( 'NONE', #23782, 1000.000000000000000 ) ;
#23022 = CARTESIAN_POINT ( 'NONE',  ( 158.0000000000011084, 98.62199963966197913, 45.00000000000000000 ) ) ;
#23023 = VECTOR ( 'NONE', #19749, 1000.000000000000000 ) ;
#23024 = PLANE ( 'NONE',  #17242 ) ;
#23025 = CARTESIAN_POINT ( 'NONE',  ( 232.4999999999996305, 83.06687458711267880, -42.88984227207694033 ) ) ;
#23026 = DIRECTION ( 'NONE',  ( -0.8916010070296632728, -0.4528218681376712240, 0.000000000000000000 ) ) ;
#23027 = CARTESIAN_POINT ( 'NONE',  ( -175.0000000000000000, -120.0000000000001705, 70.00000000000001421 ) ) ;
#23028 = ADVANCED_FACE ( 'NONE', ( #13212 ), #22245, .F. ) ;
#23029 = DIRECTION ( 'NONE',  ( 0.000000000000000000, -1.000000000000000000, 0.000000000000000000 ) ) ;
#23030 = CARTESIAN_POINT ( 'NONE',  ( -185.8971396743188791, 105.9914516682979126, -32.39061618393369457 ) ) ;
#23031 = ORIENTED_EDGE ( 'NONE', *, *, #24597, .F. ) ;
#23032 = PLANE ( 'NONE',  #11874 ) ;
#23033 = PLANE ( 'NONE',  #20215 ) ;
#23034 = CYLINDRICAL_SURFACE ( 'NONE', #11576, 5.000000000000004441 ) ;
#23035 = CARTESIAN_POINT ( 'NONE',  ( 79.99999999999990052, 230.0000000000000284, -15.00000000000000000 ) ) ;
#23036 = ORIENTED_EDGE ( 'NONE', *, *, #11870, .T. ) ;
#23037 = CARTESIAN_POINT ( 'NONE',  ( 158.0000000000014211, 73.03537455708450921, -45.00000000000000000 ) ) ;
#23038 = ORIENTED_EDGE ( 'NONE', *, *, #26233, .F. ) ;
#23039 = EDGE_CURVE ( 'NONE', #7688, #22164, #17649, .T. ) ;
#23040 = VECTOR ( 'NONE', #27853, 1000.000000000000000 ) ;
#23041 = DIRECTION ( 'NONE',  ( 0.000000000000000000, 0.000000000000000000, 1.000000000000000000 ) ) ;
#23042 = CARTESIAN_POINT ( 'NONE',  ( 119.9999999999999147, 140.0000000000000000, -100.0000000000000142 ) ) ;
#23043 = DIRECTION ( 'NONE',  ( 1.000000000000000000, 0.000000000000000000, 0.000000000000000000 ) ) ;
#23044 = ORIENTED_EDGE ( 'NONE', *, *, #12998, .F. ) ;
#23045 = PLANE ( 'NONE',  #8339 ) ;
#23046 = DIRECTION ( 'NONE',  ( 1.000000000000000000, 0.000000000000000000, 0.000000000000000000 ) ) ;
#23047 = VECTOR ( 'NONE', #24516, 1000.000000000000114 ) ;
#23048 = ORIENTED_EDGE ( 'NONE', *, *, #5240, .F. ) ;
#23049 = PRODUCT_DEFINITION_FORMATION_WITH_SPECIFIED_SOURCE ( 'ANY', '', #28144, .NOT_KNOWN. ) ;
#23050 = VECTOR ( 'NONE', #4239, 1000.000000000000000 ) ;
#23051 = CARTESIAN_POINT ( 'NONE',  ( -136.9485176461679998, 127.8960360072517801, 17.54782681003734268 ) ) ;
#23052 = CARTESIAN_POINT ( 'NONE',  ( 158.0000000000001137, 193.9212499249295831, 45.00000000000000000 ) ) ;
#23053 = ORIENTED_EDGE ( 'NONE', *, *, #5342, .F. ) ;
#23054 = EDGE_LOOP ( 'NONE', ( #27079, #7011, #3594, #20616 ) ) ;
#23055 = CARTESIAN_POINT ( 'NONE',  ( 157.4751130497510303, 215.0130877889310455, 45.00000000000000000 ) ) ;
#23056 = EDGE_LOOP ( 'NONE', ( #23263, #25570 ) ) ;
#23057 = EDGE_CURVE ( 'NONE', #19401, #7480, #9813, .T. ) ;
#23058 = EDGE_CURVE ( 'NONE', #16902, #9313, #27120, .T. ) ;
#23059 = ORIENTED_EDGE ( 'NONE', *, *, #17154, .F. ) ;
#23060 = ORIENTED_EDGE ( 'NONE', *, *, #8874, .F. ) ;
#23061 = VECTOR ( 'NONE', #9320, 1000.000000000000000 ) ;
#23062 = DIRECTION ( 'NONE',  ( 1.000000000000000000, 0.000000000000000000, -0.000000000000000000 ) ) ;
#23063 = VECTOR ( 'NONE', #24069, 1000.000000000000000 ) ;
#23064 = DIRECTION ( 'NONE',  ( -0.000000000000000000, -0.000000000000000000, -1.000000000000000000 ) ) ;
#23065 = CARTESIAN_POINT ( 'NONE',  ( 109.9999999999999574, -120.0000000000000426, 100.0000000000000142 ) ) ;
#23066 = VECTOR ( 'NONE', #27682, 999.9999999999998863 ) ;
#23067 = EDGE_CURVE ( 'NONE', #26048, #3858, #26842, .T. ) ;
#23068 = AXIS2_PLACEMENT_3D ( 'NONE', #10121, #21021, #19294 ) ;
#23069 = CARTESIAN_POINT ( 'NONE',  ( 84.91648909967481984, 110.3843228249420321, -70.37109374985145394 ) ) ;
#23070 = CARTESIAN_POINT ( 'NONE',  ( 122.6339745962154808, 239.4185842870417389, -45.00000000000000000 ) ) ;
#23071 = CARTESIAN_POINT ( 'NONE',  ( -115.3221550338875687, 71.54464929955099706, 83.00000000000001421 ) ) ;
#23072 = ADVANCED_FACE ( 'NONE', ( #24689 ), #7985, .F. ) ;
#23073 = DIRECTION ( 'NONE',  ( 0.4163300014277677707, -0.9092135777204137792, 0.000000000000000000 ) ) ;
#23074 = DIRECTION ( 'NONE',  ( 0.000000000000000000, -1.000000000000000000, 0.000000000000000000 ) ) ;
#23075 = DIRECTION ( 'NONE',  ( 0.4528218681370311249, -0.8916010070299883461, 0.000000000000000000 ) ) ;
#23076 = DIRECTION ( 'NONE',  ( 0.000000000000000000, -0.000000000000000000, 1.000000000000000000 ) ) ;
#23077 = EDGE_LOOP ( 'NONE', ( #24646, #15437, #15853, #17348 ) ) ;
#23078 = CARTESIAN_POINT ( 'NONE',  ( -23.64180107668250486, 129.3206000201379879, 15.61667362249785818 ) ) ;
#23079 = CARTESIAN_POINT ( 'NONE',  ( 157.9999999999997158, 258.6181251126050711, -45.00000000000000000 ) ) ;
#23080 = CARTESIAN_POINT ( 'NONE',  ( 79.99999999999990052, 230.0000000000000284, -5.000000000000002665 ) ) ;
#23081 = EDGE_CURVE ( 'NONE', #3367, #8626, #20230, .T. ) ;
#23082 = DIRECTION ( 'NONE',  ( 0.000000000000000000, 0.000000000000000000, 1.000000000000000000 ) ) ;
#23083 = CARTESIAN_POINT ( 'NONE',  ( -73.01279441628793165, 126.4618695315959087, 45.00000000000000000 ) ) ;
#23084 = ORIENTED_EDGE ( 'NONE', *, *, #23656, .T. ) ;
#23085 = TOROIDAL_SURFACE ( 'NONE', #613, 7.509856658345970715, 10.53396790234564762 ) ;
#23086 = AXIS2_PLACEMENT_3D ( 'NONE', #25061, #23041, #20737 ) ;
#23087 = LINE ( 'NONE', #3392, #8853 ) ;
#23088 = VERTEX_POINT ( 'NONE', #14071 ) ;
#23089 = CARTESIAN_POINT ( 'NONE',  ( 157.9999999999996874, 269.1575001501400379, -45.00000000000000000 ) ) ;
#23090 = VERTEX_POINT ( 'NONE', #11488 ) ;
#23091 = VECTOR ( 'NONE', #26377, 1000.000000000000000 ) ;
#23092 = ORIENTED_EDGE ( 'NONE', *, *, #23956, .F. ) ;
#23093 = AXIS2_PLACEMENT_3D ( 'NONE', #113, #9164, #8878 ) ;
#23094 = VERTEX_POINT ( 'NONE', #561 ) ;
#23095 = EDGE_LOOP ( 'NONE', ( #7793, #5928, #309, #27822 ) ) ;
#23096 = ORIENTED_EDGE ( 'NONE', *, *, #5580, .T. ) ;
#23097 = CARTESIAN_POINT ( 'NONE',  ( 113.1867617905505625, 214.4608731583509496, 97.32202223992300105 ) ) ;
#23098 = PLANE ( 'NONE',  #8618 ) ;
#23099 = DIRECTION ( 'NONE',  ( -1.000000000000000000, 0.000000000000000000, 0.000000000000000000 ) ) ;
#23100 = CARTESIAN_POINT ( 'NONE',  ( 158.0000000000016200, 52.97237449702815582, 45.00000000000000000 ) ) ;
#23101 = VECTOR ( 'NONE', #26266, 1000.000000000000114 ) ;
#23102 = DIRECTION ( 'NONE',  ( 0.000000000000000000, 0.000000000000000000, -1.000000000000000000 ) ) ;
#23103 = LINE ( 'NONE', #16365, #867 ) ;
#23104 = DIRECTION ( 'NONE',  ( 0.8916010070295616874, 0.4528218681378710087, 0.000000000000000000 ) ) ;
#23105 = TOROIDAL_SURFACE ( 'NONE', #11661, 45.00000000000000711, 5.000000000000000000 ) ;
#23106 = LINE ( 'NONE', #7314, #1195 ) ;
#23107 = CARTESIAN_POINT ( 'NONE',  ( -266.0448161382843182, -170.9309335098052145, -94.61759932200439493 ) ) ;
#23108 = VECTOR ( 'NONE', #1376, 1000.000000000000000 ) ;
#23109 = CYLINDRICAL_SURFACE ( 'NONE', #22074, 6.000000000000032863 ) ;
#23110 = DIRECTION ( 'NONE',  ( 0.4528218681382786270, -0.8916010070293547418, 0.000000000000000000 ) ) ;
#23111 = DIRECTION ( 'NONE',  ( -1.000000000000000000, 0.000000000000000000, 0.000000000000000000 ) ) ;
#23112 = ORIENTED_EDGE ( 'NONE', *, *, #8775, .F. ) ;
#23113 = EDGE_CURVE ( 'NONE', #12854, #61, #20086, .T. ) ;
#23114 = CARTESIAN_POINT ( 'NONE',  ( -35.14662420382099128, -18.36872720267034254, 100.0000000000000142 ) ) ;
#23115 = CARTESIAN_POINT ( 'NONE',  ( -189.6856883378720795, 103.4044969352196546, 32.84415653362697896 ) ) ;
#23116 = CARTESIAN_POINT ( 'NONE',  ( -24.92338318254761020, 127.6681916698425567, -145.0000000000000000 ) ) ;
#23118 = ORIENTED_EDGE ( 'NONE', *, *, #9436, .F. ) ;
#23117 = VERTEX_POINT ( 'NONE', #13790 ) ;
#23119 = CARTESIAN_POINT ( 'NONE',  ( 157.4999999999998579, 176.1121873686267350, 45.00000000000000000 ) ) ;
#23120 = VERTEX_POINT ( 'NONE', #20376 ) ;
#23121 = ORIENTED_EDGE ( 'NONE', *, *, #22345, .T. ) ;
#23122 = VECTOR ( 'NONE', #9400, 1000.000000000000000 ) ;
#23123 = VERTEX_POINT ( 'NONE', #15804 ) ;
#23124 = VERTEX_POINT ( 'NONE', #3121 ) ;
#23125 = VECTOR ( 'NONE', #26026, 999.9999999999998863 ) ;
#23126 = EDGE_LOOP ( 'NONE', ( #5531, #17215, #19986, #19474 ) ) ;
#23127 = DIRECTION ( 'NONE',  ( 0.4528218681380102306, -0.8916010070294909662, 0.000000000000000000 ) ) ;
#23128 = CARTESIAN_POINT ( 'NONE',  ( 217.4999999999996305, 133.0668745871126930, -36.86484227207694886 ) ) ;
#23129 = EDGE_CURVE ( 'NONE', #6895, #5063, #25854, .T. ) ;
#23130 = DIRECTION ( 'NONE',  ( -1.530283246943720875E-16, 1.000000000000000000, -0.000000000000000000 ) ) ;
#23131 = DIRECTION ( 'NONE',  ( 0.000000000000000000, 0.000000000000000000, -1.000000000000000000 ) ) ;
#23132 = CARTESIAN_POINT ( 'NONE',  ( -11.25164642577565033, 130.1410301030969663, -16.65746621873669397 ) ) ;
#23133 = DIRECTION ( 'NONE',  ( 0.000000000000000000, 0.000000000000000000, -1.000000000000000000 ) ) ;
#23134 = EDGE_CURVE ( 'NONE', #5759, #3645, #21284, .T. ) ;
#23135 = DIRECTION ( 'NONE',  ( -1.000000000000000000, 0.000000000000000000, -0.000000000000000000 ) ) ;
#23136 = CARTESIAN_POINT ( 'NONE',  ( -221.2300551840314711, 71.39986350410367777, -20.78524708593021941 ) ) ;
#23137 = AXIS2_PLACEMENT_3D ( 'NONE', #24584, #8646, #19701 ) ;
#23138 = EDGE_CURVE ( 'NONE', #9116, #12431, #9179, .T. ) ;
#23139 = ADVANCED_FACE ( 'NONE', ( #7167 ), #14409, .T. ) ;
#23140 = CARTESIAN_POINT ( 'NONE',  ( 112.4153400233872162, 200.2531221032099609, -146.5522648598509647 ) ) ;
#23141 = EDGE_CURVE ( 'NONE', #26924, #2611, #2845, .T. ) ;
#23142 = DIRECTION ( 'NONE',  ( 0.000000000000000000, -0.000000000000000000, 1.000000000000000000 ) ) ;
#23143 = CARTESIAN_POINT ( 'NONE',  ( 157.9999999999999147, 215.9842499849850697, 45.00000000000000000 ) ) ;
#23144 = DIRECTION ( 'NONE',  ( -1.000000000000000000, 0.000000000000000000, -0.000000000000000000 ) ) ;
#23145 = AXIS2_PLACEMENT_3D ( 'NONE', #8417, #3813, #13025 ) ;
#23146 = ORIENTED_EDGE ( 'NONE', *, *, #25091, .T. ) ;
#23147 = CARTESIAN_POINT ( 'NONE',  ( -200.0664673763980943, 95.37061492405908325, 31.11141022391927535 ) ) ;
#23148 = FACE_OUTER_BOUND ( 'NONE', #19486, .T. ) ;
#23149 = VERTEX_POINT ( 'NONE', #14209 ) ;
#23150 = VERTEX_POINT ( 'NONE', #26688 ) ;
#23151 = ORIENTED_EDGE ( 'NONE', *, *, #17927, .F. ) ;
#23152 = CARTESIAN_POINT ( 'NONE',  ( 119.9999999999999147, 140.0000000000000000, 100.0000000000000142 ) ) ;
#23153 = CARTESIAN_POINT ( 'NONE',  ( 0.6601832576049863066, 1.249999999999999556, 7.428391153593998375 ) ) ;
#23154 = ORIENTED_EDGE ( 'NONE', *, *, #18917, .T. ) ;
#23155 = VECTOR ( 'NONE', #27562, 1000.000000000000000 ) ;
#23156 = ORIENTED_EDGE ( 'NONE', *, *, #4998, .F. ) ;
#23157 = CARTESIAN_POINT ( 'NONE',  ( 84.91648909967481984, 110.3843228249420321, -70.37109374985145394 ) ) ;
#23158 = CARTESIAN_POINT ( 'NONE',  ( 109.9999999999999005, 260.0000000000000000, 45.00000000000000000 ) ) ;
#23159 = CARTESIAN_POINT ( 'NONE',  ( -210.0000000000000853, -213.8933171992502196, -90.09368185681015007 ) ) ;
#23160 = EDGE_LOOP ( 'NONE', ( #5674, #4071, #23289, #20402 ) ) ;
#23161 = LINE ( 'NONE', #25583, #22905 ) ;
#23162 = ORIENTED_EDGE ( 'NONE', *, *, #5240, .T. ) ;
#23163 = VECTOR ( 'NONE', #13402, 1000.000000000000000 ) ;
#23164 = DIRECTION ( 'NONE',  ( -1.000000000000000000, -0.000000000000000000, -0.000000000000000000 ) ) ;
#23165 = ADVANCED_FACE ( 'NONE', ( #11636 ), #9751, .F. ) ;
#23166 = EDGE_CURVE ( 'NONE', #26679, #19624, #22957, .T. ) ;
#23167 = CARTESIAN_POINT ( 'NONE',  ( -17.24491960465746132, 75.97823757117562593, 95.00000000000000000 ) ) ;
#23168 = FACE_OUTER_BOUND ( 'NONE', #24719, .T. ) ;
#23169 = CARTESIAN_POINT ( 'NONE',  ( 141.9187638636471434, 198.0425250404537678, 45.00000000000000000 ) ) ;
#23170 = DIRECTION ( 'NONE',  ( 0.4528218681382713551, 0.8916010070293584056, -0.000000000000000000 ) ) ;
#23171 = DIRECTION ( 'NONE',  ( -0.000000000000000000, -1.000000000000000000, -0.000000000000000000 ) ) ;
#23172 = CARTESIAN_POINT ( 'NONE',  ( 163.2529665854376333, 209.9107191942472355, -142.3325995572698446 ) ) ;
#23173 = ORIENTED_EDGE ( 'NONE', *, *, #14243, .T. ) ;
#23174 = CARTESIAN_POINT ( 'NONE',  ( 167.4999999999996589, 526.4263741777961059, -84.99999999999995737 ) ) ;
#23175 = EDGE_CURVE ( 'NONE', #26642, #10685, #1146, .T. ) ;
#23176 = AXIS2_PLACEMENT_3D ( 'NONE', #4818, #25079, #22503 ) ;
#23177 = FACE_OUTER_BOUND ( 'NONE', #11724, .T. ) ;
#23178 = DIRECTION ( 'NONE',  ( 1.000000000000000000, -0.000000000000000000, -0.000000000000000000 ) ) ;
#23179 = CARTESIAN_POINT ( 'NONE',  ( -175.0000000000000000, -120.0000000000001847, -76.02499999999999147 ) ) ;
#23180 = VERTEX_POINT ( 'NONE', #12723 ) ;
#23181 = VECTOR ( 'NONE', #17908, 1000.000000000000000 ) ;
#23182 = CARTESIAN_POINT ( 'NONE',  ( -241.9743096803475453, -91.18033988749901653, 0.000000000000000000 ) ) ;
#23183 = ORIENTED_EDGE ( 'NONE', *, *, #664, .F. ) ;
#23184 = CARTESIAN_POINT ( 'NONE',  ( 157.9999999999996589, 281.1890001801680796, -45.00000000000000000 ) ) ;
#23185 = FACE_OUTER_BOUND ( 'NONE', #22947, .T. ) ;
#23186 = CARTESIAN_POINT ( 'NONE',  ( -28.05246235954390244, 188.0718642840173516, -13.00000000000000000 ) ) ;
#23187 = ORIENTED_EDGE ( 'NONE', *, *, #17778, .F. ) ;
#23188 = DIRECTION ( 'NONE',  ( -0.000000000000000000, -0.000000000000000000, -1.000000000000000000 ) ) ;
#23189 = CARTESIAN_POINT ( 'NONE',  ( 158.0000000000008242, 128.2086247222394206, 45.00000000000000000 ) ) ;
#23190 = VECTOR ( 'NONE', #887, 1000.000000000000000 ) ;
#23191 = ORIENTED_EDGE ( 'NONE', *, *, #23297, .T. ) ;
#23192 = DIRECTION ( 'NONE',  ( -0.8916010070293483025, -0.4528218681382912281, 0.000000000000000000 ) ) ;
#23193 = DIRECTION ( 'NONE',  ( -0.000000000000000000, -0.000000000000000000, -1.000000000000000000 ) ) ;
#23194 = VERTEX_POINT ( 'NONE', #12585 ) ;
#23195 = VERTEX_POINT ( 'NONE', #14729 ) ;
#23196 = LINE ( 'NONE', #25347, #7660 ) ;
#23197 = VERTEX_POINT ( 'NONE', #5954 ) ;
#23198 = EDGE_LOOP ( 'NONE', ( #26797, #7997, #12767, #22348 ) ) ;
#23199 = ORIENTED_EDGE ( 'NONE', *, *, #13382, .F. ) ;
#23200 = VECTOR ( 'NONE', #24943, 1000.000000000000000 ) ;
#23201 = AXIS2_PLACEMENT_3D ( 'NONE', #10724, #8986, #19899 ) ;
#23202 = CARTESIAN_POINT ( 'NONE',  ( 109.8202728674729656, 257.1791079647171614, 41.57776855479137623 ) ) ;
#23204 = EDGE_CURVE ( 'NONE', #16446, #11698, #21323, .T. ) ;
#23203 = VECTOR ( 'NONE', #27881, 1000.000000000000000 ) ;
#23205 = CARTESIAN_POINT ( 'NONE',  ( 158.0000000000015632, 55.98812451204224061, 45.00000000000000000 ) ) ;
#23206 = CARTESIAN_POINT ( 'NONE',  ( 232.4999999999996305, 133.0668745871126930, 36.86484227207694886 ) ) ;
#23207 = VECTOR ( 'NONE', #18829, 1000.000000000000000 ) ;
#23208 = LINE ( 'NONE', #25632, #9658 ) ;
#23209 = CYLINDRICAL_SURFACE ( 'NONE', #13124, 16.46313063346208239 ) ;
#23210 = LINE ( 'NONE', #12166, #7471 ) ;
#23211 = DIRECTION ( 'NONE',  ( -0.8916010070293409751, -0.4528218681383056610, 0.000000000000000000 ) ) ;
#23212 = CARTESIAN_POINT ( 'NONE',  ( 157.4999999999998579, 143.5098122710352015, 45.00000000000000000 ) ) ;
#23213 = CARTESIAN_POINT ( 'NONE',  ( -210.0000000000000568, -152.0000000000000284, 105.0000000000000284 ) ) ;
#23214 = PLANE ( 'NONE',  #3345 ) ;
#23215 = EDGE_LOOP ( 'NONE', ( #6524, #21487, #27553, #4590 ) ) ;
#23216 = LINE ( 'NONE', #25369, #27448 ) ;
#23217 = EDGE_CURVE ( 'NONE', #28119, #11333, #10739, .T. ) ;
#23218 = EDGE_CURVE ( 'NONE', #761, #26048, #3532, .T. ) ;
#23219 = CARTESIAN_POINT ( 'NONE',  ( 89.99999999999988631, 240.0000000000000284, -6.270166537926030514 ) ) ;
#23220 = CARTESIAN_POINT ( 'NONE',  ( 11.04815889348632041, 90.00000000000004263, 98.28427124746193044 ) ) ;
#23221 = AXIS2_PLACEMENT_3D ( 'NONE', #18233, #14347, #23104 ) ;
#23222 = PRESENTATION_STYLE_ASSIGNMENT (( #16619 ) ) ;
#23223 = DIRECTION ( 'NONE',  ( 0.000000000000000000, -1.000000000000000000, 0.000000000000000000 ) ) ;
#23224 = ORIENTED_EDGE ( 'NONE', *, *, #16118, .T. ) ;
#23225 = AXIS2_PLACEMENT_3D ( 'NONE', #1172, #10362, #9942 ) ;
#23226 = DIRECTION ( 'NONE',  ( -0.000000000000000000, -0.000000000000000000, -1.000000000000000000 ) ) ;
#23227 = ORIENTED_EDGE ( 'NONE', *, *, #7865, .F. ) ;
#23228 = PLANE ( 'NONE',  #4816 ) ;
#23229 = ORIENTED_EDGE ( 'NONE', *, *, #9909, .F. ) ;
#23230 = AXIS2_PLACEMENT_3D ( 'NONE', #20381, #12058, #22688 ) ;
#23231 = EDGE_CURVE ( 'NONE', #19001, #16156, #27912, .T. ) ;
#23232 = ORIENTED_EDGE ( 'NONE', *, *, #18603, .T. ) ;
#23233 = CARTESIAN_POINT ( 'NONE',  ( -67.48155814317149748, 135.5182078837663369, 13.65863916513348997 ) ) ;
#23234 = ADVANCED_FACE ( 'NONE', ( #8258, #9887 ), #8401, .F. ) ;
#23235 = APPLICATION_CONTEXT ( 'automotive_design' ) ;
#23236 = VERTEX_POINT ( 'NONE', #21461 ) ;
#23237 = ORIENTED_EDGE ( 'NONE', *, *, #8847, .F. ) ;
#23238 = CARTESIAN_POINT ( 'NONE',  ( 113.9305603607157025, 227.9104510466760303, 97.95022080735130032 ) ) ;
#23239 = DIRECTION ( 'NONE',  ( 0.000000000000000000, 1.000000000000000000, 0.000000000000000000 ) ) ;
#23240 = CARTESIAN_POINT ( 'NONE',  ( 79.99999999999994316, -100.0000000000000284, 100.0000000000000142 ) ) ;
#23241 = FACE_OUTER_BOUND ( 'NONE', #20985, .T. ) ;
#23242 = CIRCLE ( 'NONE', #22800, 5.999999999999977796 ) ;
#23243 = DIRECTION ( 'NONE',  ( -0.000000000000000000, 0.000000000000000000, 1.000000000000000000 ) ) ;
#23244 = PLANE ( 'NONE',  #12342 ) ;
#23245 = CARTESIAN_POINT ( 'NONE',  ( -272.7483281375958200, -170.1453890489109142, 92.73246688958286654 ) ) ;
#23246 = CARTESIAN_POINT ( 'NONE',  ( 129.3069818644945883, 249.4552694810368507, -146.9347961558894724 ) ) ;
#23247 = CARTESIAN_POINT ( 'NONE',  ( -261.1919288306253293, -171.9377729149742038, -104.9999999999998721 ) ) ;
#23248 = CARTESIAN_POINT ( 'NONE',  ( 158.0000000000008527, 125.7007497147323818, 45.00000000000000000 ) ) ;
#23249 = DIRECTION ( 'NONE',  ( 0.8916010070293562961, 0.4528218681382754629, -0.000000000000000000 ) ) ;
#23250 = CARTESIAN_POINT ( 'NONE',  ( 157.9999999999997158, 263.6338751276190351, -45.00000000000000000 ) ) ;
#23251 = ORIENTED_EDGE ( 'NONE', *, *, #24565, .F. ) ;
#23252 = ADVANCED_FACE ( 'NONE', ( #8681 ), #6237, .T. ) ;
#23253 = EDGE_CURVE ( 'NONE', #3880, #21558, #28336, .T. ) ;
#23254 = CARTESIAN_POINT ( 'NONE',  ( -46.68942599940377391, -18.01420295945611727, 100.0000000000000000 ) ) ;
#23255 = CARTESIAN_POINT ( 'NONE',  ( 157.9999999999996305, 288.7126252026890256, 45.00000000000000000 ) ) ;
#23257 = VERTEX_POINT ( 'NONE', #19312 ) ;
#23256 = EDGE_LOOP ( 'NONE', ( #18422, #23084, #4335, #8702 ) ) ;
#23258 = DIRECTION ( 'NONE',  ( -0.9506505318133544602, -0.3102637045530566295, 0.000000000000000000 ) ) ;
#23259 = ORIENTED_EDGE ( 'NONE', *, *, #10977, .T. ) ;
#23260 = ORIENTED_EDGE ( 'NONE', *, *, #14087, .T. ) ;
#23261 = VECTOR ( 'NONE', #3044, 1000.000000000000000 ) ;
#23262 = ADVANCED_FACE ( 'NONE', ( #28055 ), #17013, .F. ) ;
#23263 = ORIENTED_EDGE ( 'NONE', *, *, #13106, .F. ) ;
#23264 = AXIS2_PLACEMENT_3D ( 'NONE', #5844, #7859, #5985 ) ;
#23265 = ORIENTED_EDGE ( 'NONE', *, *, #10174, .F. ) ;
#23266 = EDGE_LOOP ( 'NONE', ( #25523, #16103, #9984, #3599 ) ) ;
#23267 = ORIENTED_EDGE ( 'NONE', *, *, #10517, .F. ) ;
#23268 = ADVANCED_FACE ( 'NONE', ( #15013 ), #23764, .F. ) ;
#23269 = CARTESIAN_POINT ( 'NONE',  ( -233.2943309833553371, 92.06151970357247194, 13.00000000000000000 ) ) ;
#23270 = EDGE_CURVE ( 'NONE', #83, #23194, #1917, .T. ) ;
#23271 = LINE ( 'NONE', #4144, #12384 ) ;
#23272 = EDGE_CURVE ( 'NONE', #24388, #24788, #28196, .T. ) ;
#23273 = DIRECTION ( 'NONE',  ( 0.000000000000000000, 1.000000000000000000, -0.000000000000000000 ) ) ;
#23274 = LINE ( 'NONE', #1573, #25238 ) ;
#23275 = DIRECTION ( 'NONE',  ( 1.000000000000000000, 0.000000000000000000, 0.000000000000000000 ) ) ;
#23276 = PLANE ( 'NONE',  #21055 ) ;
#23277 = CIRCLE ( 'NONE', #16417, 6.000000000000005329 ) ;
#23278 = CARTESIAN_POINT ( 'NONE',  ( -194.2411556039511709, 63.21395545898181467, -45.39084185613187827 ) ) ;
#23279 = LINE ( 'NONE', #27428, #15089 ) ;
#23280 = CARTESIAN_POINT ( 'NONE',  ( 79.99999999999991473, 140.0000000000000000, -45.00000000000000000 ) ) ;
#23281 = CARTESIAN_POINT ( 'NONE',  ( -270.1025481742786951, -91.18033988749901653, 11.42311362948588105 ) ) ;
#23282 = LINE ( 'NONE', #14386, #23040 ) ;
#23283 = VERTEX_POINT ( 'NONE', #19594 ) ;
#23284 = PLANE ( 'NONE',  #15582 ) ;
#23285 = CARTESIAN_POINT ( 'NONE',  ( -229.2498027451138967, 132.0565166830976978, -15.00000000000000000 ) ) ;
#23286 = ORIENTED_EDGE ( 'NONE', *, *, #983, .T. ) ;
#23287 = SHAPE_DEFINITION_REPRESENTATION ( #17379, #11963 ) ;
#23288 = EDGE_LOOP ( 'NONE', ( #7189, #267, #9824, #17802 ) ) ;
#23289 = ORIENTED_EDGE ( 'NONE', *, *, #16972, .F. ) ;
#23290 = AXIS2_PLACEMENT_3D ( 'NONE', #4181, #10806, #19563 ) ;
#23291 = CARTESIAN_POINT ( 'NONE',  ( 95.20156243614241021, 83.09913198708241566, 100.0000000000000142 ) ) ;
#23292 = LINE ( 'NONE', #12394, #6705 ) ;
#23293 = VERTEX_POINT ( 'NONE', #26193 ) ;
#23294 = EDGE_CURVE ( 'NONE', #14508, #8985, #12054, .T. ) ;
#23295 = ORIENTED_EDGE ( 'NONE', *, *, #17888, .T. ) ;
#23296 = PLANE ( 'NONE',  #5377 ) ;
#23297 = EDGE_CURVE ( 'NONE', #883, #11955, #11117, .T. ) ;
#23298 = CARTESIAN_POINT ( 'NONE',  ( 132.3894761555990556, 200.1711027725235397, -45.00000000000000000 ) ) ;
#23299 = EDGE_CURVE ( 'NONE', #729, #26043, #2479, .T. ) ;
#23300 = DIRECTION ( 'NONE',  ( 1.000000000000000000, 0.000000000000000000, -0.000000000000000000 ) ) ;
#23301 = ORIENTED_EDGE ( 'NONE', *, *, #24046, .T. ) ;
#23302 = CARTESIAN_POINT ( 'NONE',  ( 119.7545560453059892, 132.4900181921427702, 100.0000000000000142 ) ) ;
#23303 = ORIENTED_EDGE ( 'NONE', *, *, #15869, .F. ) ;
#23304 = DIRECTION ( 'NONE',  ( 1.000000000000000000, -0.000000000000000000, -0.000000000000000000 ) ) ;
#23305 = CARTESIAN_POINT ( 'NONE',  ( 158.0000000000002558, 183.3818748873943889, 45.00000000000000000 ) ) ;
#23306 = CARTESIAN_POINT ( 'NONE',  ( 157.4999999999998579, 70.78143705333094715, 45.00000000000000000 ) ) ;
#23307 = DIRECTION ( 'NONE',  ( 1.000000000000000000, 0.000000000000000000, 2.775557561562887407E-16 ) ) ;
#23308 = DIRECTION ( 'NONE',  ( 0.000000000000000000, 0.000000000000000000, -1.000000000000000000 ) ) ;
#23309 = CARTESIAN_POINT ( 'NONE',  ( 134.9999999999998579, 457.0747856552986832, -145.0000000000000000 ) ) ;
#23310 = CARTESIAN_POINT ( 'NONE',  ( 163.4434812112566249, 210.4619483375885238, -145.7833319456713639 ) ) ;
#23311 = AXIS2_PLACEMENT_3D ( 'NONE', #7318, #17945, #16093 ) ;
#23312 = ORIENTED_EDGE ( 'NONE', *, *, #12866, .T. ) ;
#23313 = CARTESIAN_POINT ( 'NONE',  ( 79.99999999999992895, 110.0000000000000000, 70.00000000000001421 ) ) ;
#23314 = VECTOR ( 'NONE', #20875, 1000.000000000000114 ) ;
#23315 = DIRECTION ( 'NONE',  ( 0.5000000000000039968, 0.8660254037844364872, 0.000000000000000000 ) ) ;
#23316 = DIRECTION ( 'NONE',  ( -0.000000000000000000, 0.000000000000000000, -1.000000000000000000 ) ) ;
#23317 = FACE_OUTER_BOUND ( 'NONE', #9282, .T. ) ;
#23318 = ORIENTED_EDGE ( 'NONE', *, *, #4957, .T. ) ;
#23319 = DIRECTION ( 'NONE',  ( -0.8916010070293485246, -0.4528218681382906730, 0.000000000000000000 ) ) ;
#23320 = ORIENTED_EDGE ( 'NONE', *, *, #15762, .F. ) ;
#23321 = CARTESIAN_POINT ( 'NONE',  ( -200.0057241004398634, 95.74183647495578953, 30.18583206540278141 ) ) ;
#23322 = DIRECTION ( 'NONE',  ( 0.000000000000000000, -0.000000000000000000, -1.000000000000000000 ) ) ;
#23323 = DIRECTION ( 'NONE',  ( -0.8916010070296834789, -0.4528218681376312005, 0.000000000000000000 ) ) ;
#23324 = ORIENTED_EDGE ( 'NONE', *, *, #26791, .F. ) ;
#23325 = CARTESIAN_POINT ( 'NONE',  ( 157.4999999999996589, 276.4271876689075498, 45.00000000000000000 ) ) ;
#23326 = ORIENTED_EDGE ( 'NONE', *, *, #27306, .F. ) ;
#23327 = EDGE_CURVE ( 'NONE', #6913, #18244, #11209, .T. ) ;
#23328 = CARTESIAN_POINT ( 'NONE',  ( 157.4999999999998579, 103.3838121509225090, 45.00000000000000000 ) ) ;
#23329 = CIRCLE ( 'NONE', #23348, 5.999999999999977796 ) ;
#23330 = LINE ( 'NONE', #12430, #275 ) ;
#23331 = ORIENTED_EDGE ( 'NONE', *, *, #17041, .F. ) ;
#23332 = EDGE_LOOP ( 'NONE', ( #1660, #24776, #11433, #11304 ) ) ;
#23333 = EDGE_CURVE ( 'NONE', #1220, #24140, #18011, .T. ) ;
#23334 = CARTESIAN_POINT ( 'NONE',  ( -210.0000000000000568, -213.8933171992501627, -109.9063181431897789 ) ) ;
#23335 = ORIENTED_EDGE ( 'NONE', *, *, #17034, .T. ) ;
#23336 = VECTOR ( 'NONE', #10144, 999.9999999999998863 ) ;
#23337 = EDGE_CURVE ( 'NONE', #18077, #4836, #4922, .T. ) ;
#23338 = VECTOR ( 'NONE', #1543, 1000.000000000000000 ) ;
#23339 = VERTEX_POINT ( 'NONE', #56 ) ;
#23340 = B_SPLINE_CURVE_WITH_KNOTS ( 'NONE', 3,
 ( #17567, #26325, #15292, #24045, #13141, #26044, #6364, #17148, #12997, #192, #24316, #21881, #2187, #1909 ),
 .UNSPECIFIED., .F., .F.,
 ( 4, 2, 2, 2, 2, 2, 4 ),
 ( 2.775557561562891351E-17, 0.001449360111607882239, 0.002174040167411816094, 0.002898720223215749733, 0.003623400279019683371, 0.004348080334823617443, 0.005797440446431482118 ),
 .UNSPECIFIED. ) ;
#23341 = ORIENTED_EDGE ( 'NONE', *, *, #9977, .T. ) ;
#23342 = DIRECTION ( 'NONE',  ( 2.775557561562887407E-16, 3.668437989309015850E-32, -1.000000000000000000 ) ) ;
#23343 = LINE ( 'NONE', #1503, #3435 ) ;
#23344 = CARTESIAN_POINT ( 'NONE',  ( 0.3999999999999999667, 0.000000000000000000, 0.000000000000000000 ) ) ;
#23345 = LINE ( 'NONE', #10415, #25712 ) ;
#23346 = DIRECTION ( 'NONE',  ( 0.8916010070295820045, -0.4528218681378310406, 0.000000000000000000 ) ) ;
#23347 = CARTESIAN_POINT ( 'NONE',  ( -225.1304350307114532, 62.42764488596311878, -8.801787756210094571 ) ) ;
#23348 = AXIS2_PLACEMENT_3D ( 'NONE', #607, #15984, #13830 ) ;
#23349 = CARTESIAN_POINT ( 'NONE',  ( 340.3127869742386338, 101.4626071723496779, -145.0000000000000000 ) ) ;
#23350 = LINE ( 'NONE', #10421, #17048 ) ;
#23351 = LINE ( 'NONE', #25638, #27882 ) ;
#23352 = PLANE ( 'NONE',  #21269 ) ;
#23353 = ORIENTED_EDGE ( 'NONE', *, *, #20447, .T. ) ;
#23354 = CARTESIAN_POINT ( 'NONE',  ( 134.9999999999998579, 404.6636166603179277, -151.0000000000000000 ) ) ;
#23355 = DIRECTION ( 'NONE',  ( -0.000000000000000000, -0.000000000000000000, -1.000000000000000000 ) ) ;
#23356 = CARTESIAN_POINT ( 'NONE',  ( 158.0000000000015064, 63.00387452705633251, -45.00000000000000000 ) ) ;
#23357 = LINE ( 'NONE', #3669, #4676 ) ;
#23358 = ORIENTED_EDGE ( 'NONE', *, *, #25514, .F. ) ;
#23359 = ADVANCED_FACE ( 'NONE', ( #20013 ), #8814, .F. ) ;
#23360 = CARTESIAN_POINT ( 'NONE',  ( -231.0630381273050489, 75.70161533889120165, 15.87871908887787953 ) ) ;
#23361 = ORIENTED_EDGE ( 'NONE', *, *, #17196, .F. ) ;
#23362 = CARTESIAN_POINT ( 'NONE',  ( 65.00000000000000000, -150.0000000000000568, -69.99999999999998579 ) ) ;
#23363 = ORIENTED_EDGE ( 'NONE', *, *, #16523, .T. ) ;
#23364 = ORIENTED_EDGE ( 'NONE', *, *, #7692, .F. ) ;
#23365 = CARTESIAN_POINT ( 'NONE',  ( -85.27503253815632434, 136.4561186087251770, 15.16277632316441881 ) ) ;
#23366 = CIRCLE ( 'NONE', #11452, 30.00000000000000000 ) ;
#23367 = EDGE_CURVE ( 'NONE', #25689, #14705, #18080, .T. ) ;
#23368 = VECTOR ( 'NONE', #11976, 1000.000000000000000 ) ;
#23369 = ORIENTED_EDGE ( 'NONE', *, *, #12611, .F. ) ;
#23370 = ORIENTED_EDGE ( 'NONE', *, *, #14741, .F. ) ;
#23371 = CARTESIAN_POINT ( 'NONE',  ( 113.6021183481338284, 226.9733193880700242, 97.68838206577115102 ) ) ;
#23372 = DIRECTION ( 'NONE',  ( 0.000000000000000000, 0.000000000000000000, 1.000000000000000000 ) ) ;
#23373 = LINE ( 'NONE', #19629, #13422 ) ;
#23374 = TOROIDAL_SURFACE ( 'NONE', #13297, 35.00000000000000711, 5.000000000000000000 ) ;
#23375 = ADVANCED_FACE ( 'NONE', ( #22031 ), #27251, .F. ) ;
#23376 = CARTESIAN_POINT ( 'NONE',  ( -134.5993320547982535, 128.5490369126959251, -17.26385867077430447 ) ) ;
#23377 = VECTOR ( 'NONE', #18400, 1000.000000000000000 ) ;
#23378 = CARTESIAN_POINT ( 'NONE',  ( -270.0655465147688687, -165.1941129551596248, -88.29030773487120598 ) ) ;
#23379 = LINE ( 'NONE', #12056, #21035 ) ;
#23380 = LINE ( 'NONE', #21081, #14509 ) ;
#23381 = CARTESIAN_POINT ( 'NONE',  ( 132.8750286730203811, 249.9251938516255791, -150.6145052419835508 ) ) ;
#23382 = CARTESIAN_POINT ( 'NONE',  ( -218.6660474811943971, 86.19516118637005775, 19.43150922036087280 ) ) ;
#23383 = CARTESIAN_POINT ( 'NONE',  ( 65.00000000000000000, -120.0250000000000909, -69.99999999999998579 ) ) ;
#23384 = DIRECTION ( 'NONE',  ( 1.000000000000000000, 0.000000000000000000, -0.000000000000000000 ) ) ;
#23385 = CARTESIAN_POINT ( 'NONE',  ( 74.37710191228967460, 227.8920494084358950, 45.00000000000000000 ) ) ;
#23386 = VERTEX_POINT ( 'NONE', #24474 ) ;
#23387 = ADVANCED_FACE ( 'NONE', ( #15576 ), #20371, .T. ) ;
#23388 = AXIS2_PLACEMENT_3D ( 'NONE', #24743, #13693, #751 ) ;
#23389 = CARTESIAN_POINT ( 'NONE',  ( -110.3221550338875687, 20.24192588826928585, 80.00000000000001421 ) ) ;
#23390 = CARTESIAN_POINT ( 'NONE',  ( 232.4999999999996305, 133.0668745871126930, -42.86484227207692044 ) ) ;
#23392 = ORIENTED_EDGE ( 'NONE', *, *, #14074, .F. ) ;
#23391 = VERTEX_POINT ( 'NONE', #24323 ) ;
#23393 = AXIS2_PLACEMENT_3D ( 'NONE', #5269, #958, #2531 ) ;
#23394 = EDGE_CURVE ( 'NONE', #5337, #23117, #9104, .T. ) ;
#23395 = CARTESIAN_POINT ( 'NONE',  ( 101.0213870967668299, 236.0005211361351485, -23.58009545578860511 ) ) ;
#23396 = AXIS2_PLACEMENT_3D ( 'NONE', #7482, #23127, #27415 ) ;
#23397 = ORIENTED_EDGE ( 'NONE', *, *, #18662, .F. ) ;
#23398 = ORIENTED_EDGE ( 'NONE', *, *, #2842, .F. ) ;
#23399 = ORIENTED_EDGE ( 'NONE', *, *, #16229, .T. ) ;
#23400 = ORIENTED_EDGE ( 'NONE', *, *, #24461, .T. ) ;
#23401 = ORIENTED_EDGE ( 'NONE', *, *, #16085, .F. ) ;
#23402 = ORIENTED_EDGE ( 'NONE', *, *, #17543, .T. ) ;
#23403 = DIRECTION ( 'NONE',  ( -0.7071067811865455743, 0.000000000000000000, 0.7071067811865493491 ) ) ;
#23404 = EDGE_CURVE ( 'NONE', #15146, #23195, #2626, .T. ) ;
#23405 = EDGE_CURVE ( 'NONE', #4212, #13878, #11563, .T. ) ;
#23406 = VECTOR ( 'NONE', #2955, 1000.000000000000227 ) ;
#23407 = LINE ( 'NONE', #12788, #26121 ) ;
#23408 = LINE ( 'NONE', #10339, #15777 ) ;
#23409 = VECTOR ( 'NONE', #12507, 1000.000000000000000 ) ;
#23410 = CARTESIAN_POINT ( 'NONE',  ( 134.0000000000000853, 196.9999999999997442, 45.00000000000000000 ) ) ;
#23411 = DIRECTION ( 'NONE',  ( 0.000000000000000000, 1.000000000000000000, 0.000000000000000000 ) ) ;
#23412 = FACE_OUTER_BOUND ( 'NONE', #6089, .T. ) ;
#23413 = CARTESIAN_POINT ( 'NONE',  ( -207.5241688850417745, 75.58432268001081411, -43.94049219536437789 ) ) ;
#23414 = ADVANCED_FACE ( 'NONE', ( #17862 ), #13148, .F. ) ;
#23415 = CARTESIAN_POINT ( 'NONE',  ( 112.1383963276659159, 200.5739753623955437, -147.6595947404202320 ) ) ;
#23416 = CARTESIAN_POINT ( 'NONE',  ( 158.0000000000014495, 68.01962454207041731, 45.00000000000000000 ) ) ;
#23417 = LINE ( 'NONE', #19678, #12911 ) ;
#23418 = LINE ( 'NONE', #21403, #22594 ) ;
#23419 = ORIENTED_EDGE ( 'NONE', *, *, #22946, .F. ) ;
#23420 = CARTESIAN_POINT ( 'NONE',  ( -203.3278902001933943, 92.92226908766612326, 29.32321494459338851 ) ) ;
#23421 = EDGE_CURVE ( 'NONE', #13130, #9383, #2337, .T. ) ;
#23422 = VECTOR ( 'NONE', #22651, 1000.000000000000000 ) ;
#23423 = DIRECTION ( 'NONE',  ( 0.000000000000000000, 0.000000000000000000, 1.000000000000000000 ) ) ;
#23424 = EDGE_LOOP ( 'NONE', ( #4157, #20735, #3749, #20933 ) ) ;
#23425 = APPLICATION_PROTOCOL_DEFINITION ( 'draft international standard', 'automotive_design', 1998, #5981 ) ;
#23426 = ADVANCED_FACE ( 'NONE', ( #2195 ), #10980, .F. ) ;
#23427 = ORIENTED_EDGE ( 'NONE', *, *, #21569, .F. ) ;
#23428 = ORIENTED_EDGE ( 'NONE', *, *, #17196, .T. ) ;
#23429 = VECTOR ( 'NONE', #19706, 1000.000000000000000 ) ;
#23430 = CARTESIAN_POINT ( 'NONE',  ( 158.0000000000015916, 53.48024950453520177, 45.00000000000000000 ) ) ;
#23431 = CARTESIAN_POINT ( 'NONE',  ( 158.0000000000002274, 183.8897498949014278, -45.00000000000000000 ) ) ;
#23432 = VERTEX_POINT ( 'NONE', #9249 ) ;
#23433 = VERTEX_POINT ( 'NONE', #199 ) ;
#23434 = FACE_OUTER_BOUND ( 'NONE', #11148, .T. ) ;
#23435 = DIRECTION ( 'NONE',  ( -0.000000000000000000, -0.000000000000000000, 1.000000000000000000 ) ) ;
#23436 = AXIS2_PLACEMENT_3D ( 'NONE', #13965, #3013, #16389 ) ;
#23437 = CARTESIAN_POINT ( 'NONE',  ( -290.0000000000001705, -220.0000000000000853, -59.99999999999987210 ) ) ;
#23438 = ORIENTED_EDGE ( 'NONE', *, *, #894, .F. ) ;
#23439 = CARTESIAN_POINT ( 'NONE',  ( -175.0000000000000000, -150.0000000000000853, -69.99999999999998579 ) ) ;
#23440 = ORIENTED_EDGE ( 'NONE', *, *, #22025, .F. ) ;
#23441 = DIRECTION ( 'NONE',  ( 0.000000000000000000, 0.000000000000000000, -1.000000000000000000 ) ) ;
#23442 = AXIS2_PLACEMENT_3D ( 'NONE', #712, #23877, #20237 ) ;
#23443 = DIRECTION ( 'NONE',  ( -0.5000000000000106581, -0.8660254037844326014, 0.000000000000000000 ) ) ;
#23444 = LINE ( 'NONE', #19419, #18563 ) ;
#23445 = DIRECTION ( 'NONE',  ( -0.000000000000000000, -0.000000000000000000, -1.000000000000000000 ) ) ;
#23446 = DIRECTION ( 'NONE',  ( 0.4528218681377111920, -0.8916010070296429557, 0.000000000000000000 ) ) ;
#23447 = CARTESIAN_POINT ( 'NONE',  ( 157.4999999999998579, 73.28931206083800021, -45.00000000000000000 ) ) ;
#23448 = AXIS2_PLACEMENT_3D ( 'NONE', #19960, #17513, #24705 ) ;
#23449 = CARTESIAN_POINT ( 'NONE',  ( 162.2129141269701620, 207.3671766611915359, -150.3892986974657617 ) ) ;
#23450 = VERTEX_POINT ( 'NONE', #26772 ) ;
#23451 = LINE ( 'NONE', #12132, #23314 ) ;
#23452 = CARTESIAN_POINT ( 'NONE',  ( 158.0000000000011084, 98.62199963966197913, -45.00000000000000000 ) ) ;
#23453 = DIRECTION ( 'NONE',  ( 1.000000000000000000, 0.000000000000000000, -0.000000000000000000 ) ) ;
#23454 = EDGE_CURVE ( 'NONE', #13425, #2326, #8960, .T. ) ;
#23455 = CARTESIAN_POINT ( 'NONE',  ( -48.38593899427829115, 148.2549133597845241, 45.00000000000000000 ) ) ;
#23456 = EDGE_LOOP ( 'NONE', ( #441, #1136, #18027, #11994 ) ) ;
#23457 = FACE_BOUND ( 'NONE', #12831, .T. ) ;
#23458 = EDGE_CURVE ( 'NONE', #11964, #24937, #6797, .T. ) ;
#23459 = EDGE_LOOP ( 'NONE', ( #14036, #20592, #2536, #28351 ) ) ;
#23460 = DIRECTION ( 'NONE',  ( -0.8916010070298665546, -0.4528218681372709331, 0.000000000000000000 ) ) ;
#23461 = DIRECTION ( 'NONE',  ( 0.000000000000000000, -1.214306433183764966E-16, 1.000000000000000000 ) ) ;
#23462 = CARTESIAN_POINT ( 'NONE',  ( -227.0732549327441632, 90.14410762487624140, 13.63207569781857131 ) ) ;
#23463 = ORIENTED_EDGE ( 'NONE', *, *, #7015, .F. ) ;
#23464 = DIRECTION ( 'NONE',  ( 0.8916010070293584056, -0.4528218681382712996, 0.000000000000000000 ) ) ;
#23465 = DIRECTION ( 'NONE',  ( 0.8916010070294301260, 0.4528218681381301347, 0.000000000000000000 ) ) ;
#23466 = VERTEX_POINT ( 'NONE', #3055 ) ;
#23467 = AXIS2_PLACEMENT_3D ( 'NONE', #16783, #25961, #12764 ) ;
#23468 = CARTESIAN_POINT ( 'NONE',  ( 139.9869122110687840, 242.4751130497508314, -45.00000000000000000 ) ) ;
#23469 = CARTESIAN_POINT ( 'NONE',  ( 113.0425250404538673, 226.9187638636466602, 45.00000000000000000 ) ) ;
#23470 = ORIENTED_EDGE ( 'NONE', *, *, #16314, .F. ) ;
#23471 = CIRCLE ( 'NONE', #22097, 34.99999999999999289 ) ;
#23472 = ORIENTED_EDGE ( 'NONE', *, *, #5750, .T. ) ;
#23473 = DIRECTION ( 'NONE',  ( 1.000000000000000000, -0.000000000000000000, -0.000000000000000000 ) ) ;
#23474 = ORIENTED_EDGE ( 'NONE', *, *, #495, .T. ) ;
#23475 = AXIS2_PLACEMENT_3D ( 'NONE', #823, #7847, #16620 ) ;
#23476 = EDGE_CURVE ( 'NONE', #17780, #8629, #27457, .T. ) ;
#23477 = ORIENTED_EDGE ( 'NONE', *, *, #13454, .T. ) ;
#23478 = ORIENTED_EDGE ( 'NONE', *, *, #9846, .F. ) ;
#23479 = FACE_OUTER_BOUND ( 'NONE', #18636, .T. ) ;
#23480 = EDGE_CURVE ( 'NONE', #12943, #1444, #16011, .T. ) ;
#23481 = DIRECTION ( 'NONE',  ( 0.000000000000000000, 0.000000000000000000, -1.000000000000000000 ) ) ;
#23482 = CARTESIAN_POINT ( 'NONE',  ( 0.03763830711997131345, 1.249999999999999556, 7.196935439755601571 ) ) ;
#23483 = FACE_OUTER_BOUND ( 'NONE', #1948, .T. ) ;
#23484 = CARTESIAN_POINT ( 'NONE',  ( 157.9999999999998295, 226.5236250225210313, 45.00000000000000000 ) ) ;
#23485 = CARTESIAN_POINT ( 'NONE',  ( 158.0000000000009663, 111.1613746771971876, 45.00000000000000000 ) ) ;
#23486 = CARTESIAN_POINT ( 'NONE',  ( -242.5499235585615452, 73.68467268309757401, -14.74213902348974159 ) ) ;
#23487 = VERTEX_POINT ( 'NONE', #14136 ) ;
#23488 = VECTOR ( 'NONE', #16438, 1000.000000000000000 ) ;
#23489 = CARTESIAN_POINT ( 'NONE',  ( 157.9999999999996305, 288.7126252026890256, 45.00000000000000000 ) ) ;
#23490 = ADVANCED_FACE ( 'NONE', ( #11704 ), #27320, .F. ) ;
#23491 = DIRECTION ( 'NONE',  ( 0.8916010070297745171, -0.4528218681374519550, 0.000000000000000000 ) ) ;
#23493 = LINE ( 'NONE', #22329, #10049 ) ;
#23492 = VECTOR ( 'NONE', #6647, 1000.000000000000000 ) ;
#23494 = CARTESIAN_POINT ( 'NONE',  ( -26.23654403271235225, 26.23654403271337543, 45.00000000000000000 ) ) ;
#23495 = ORIENTED_EDGE ( 'NONE', *, *, #11568, .F. ) ;
#23496 = EDGE_CURVE ( 'NONE', #15403, #1139, #11981, .T. ) ;
#23497 = DIRECTION ( 'NONE',  ( 0.000000000000000000, -1.000000000000000000, 0.000000000000000000 ) ) ;
#23498 = EDGE_CURVE ( 'NONE', #12493, #2404, #25319, .T. ) ;
#23499 = PLANE ( 'NONE',  #14225 ) ;
#23500 = CARTESIAN_POINT ( 'NONE',  ( -156.2917263574996127, 178.8555734514394828, -15.00000000000000000 ) ) ;
#23501 = DIRECTION ( 'NONE',  ( 1.000000000000000000, 0.000000000000000000, 0.000000000000000000 ) ) ;
#23502 = LINE ( 'NONE', #3953, #8363 ) ;
#23503 = VERTEX_POINT ( 'NONE', #27598 ) ;
#23504 = CARTESIAN_POINT ( 'NONE',  ( -234.3977820475819840, 78.94297905343258037, 15.16298856074166679 ) ) ;
#23505 = ORIENTED_EDGE ( 'NONE', *, *, #12508, .T. ) ;
#23506 = DIRECTION ( 'NONE',  ( 0.2588190451025286221, 0.9659258262890662028, 0.000000000000000000 ) ) ;
#23507 = VERTEX_POINT ( 'NONE', #1048 ) ;
#23508 = EDGE_LOOP ( 'NONE', ( #3962, #21912, #4192 ) ) ;
#23509 = LINE ( 'NONE', #3824, #8563 ) ;
#23510 = EDGE_LOOP ( 'NONE', ( #17032, #21981, #10161, #14444 ) ) ;
#23511 = ORIENTED_EDGE ( 'NONE', *, *, #1428, .T. ) ;
#23512 = VECTOR ( 'NONE', #10140, 1000.000000000000114 ) ;
#23513 = CARTESIAN_POINT ( 'NONE',  ( 157.4999999999997726, 243.8248125713165280, 45.00000000000000000 ) ) ;
#23514 = DIRECTION ( 'NONE',  ( -0.8916010070295719014, -0.4528218681378510246, 0.000000000000000000 ) ) ;
#23515 = CARTESIAN_POINT ( 'NONE',  ( 157.4999999999998579, 148.5255622860493077, 45.00000000000000000 ) ) ;
#23516 = CIRCLE ( 'NONE', #15740, 18.46313063346208239 ) ;
#23517 = CARTESIAN_POINT ( 'NONE',  ( -122.5485268256659594, 131.3750725269259476, -16.25384529279319779 ) ) ;
#23518 = EDGE_CURVE ( 'NONE', #17397, #1528, #6173, .T. ) ;
#23519 = CARTESIAN_POINT ( 'NONE',  ( -260.0000000000001137, -167.0819201924624906, -89.99999999999987210 ) ) ;
#23520 = PLANE ( 'NONE',  #14628 ) ;
#23521 = EDGE_CURVE ( 'NONE', #17245, #10183, #25875, .T. ) ;
#23522 = CARTESIAN_POINT ( 'NONE',  ( 187.4999999999996305, 133.0668745871126930, -30.86484227207697018 ) ) ;
#23523 = CARTESIAN_POINT ( 'NONE',  ( -229.2280533001591607, 91.38976949163449603, -15.26004308210696792 ) ) ;
#23524 = DIRECTION ( 'NONE',  ( 0.000000000000000000, 0.000000000000000000, -1.000000000000000000 ) ) ;
#23525 = EDGE_CURVE ( 'NONE', #3222, #5588, #13993, .T. ) ;
#23526 = CARTESIAN_POINT ( 'NONE',  ( -227.9935532272682508, 88.33663008737792666, 15.67459936273962384 ) ) ;
#23527 = CARTESIAN_POINT ( 'NONE',  ( 157.4999999999994600, 213.7303124812313513, 45.00000000000000000 ) ) ;
#23528 = LINE ( 'NONE', #21227, #18259 ) ;
#23529 = DIRECTION ( 'NONE',  ( 1.000000000000000000, 0.000000000000000000, 0.000000000000000000 ) ) ;
#23530 = VERTEX_POINT ( 'NONE', #18299 ) ;
#23531 = VECTOR ( 'NONE', #12960, 1000.000000000000000 ) ;
#23532 = AXIS2_PLACEMENT_3D ( 'NONE', #1656, #14222, #8558 ) ;
#23533 = EDGE_CURVE ( 'NONE', #27901, #19692, #3194, .T. ) ;
#23534 = DIRECTION ( 'NONE',  ( -0.000000000000000000, -0.000000000000000000, 1.000000000000000000 ) ) ;
#23535 = DIRECTION ( 'NONE',  ( 0.8916010070293409751, 0.4528218681383056610, 0.000000000000000000 ) ) ;
#23536 = CARTESIAN_POINT ( 'NONE',  ( 65.00000000000000000, -120.0250000000000625, 70.00000000000001421 ) ) ;
#23537 = AXIS2_PLACEMENT_3D ( 'NONE', #24844, #26988, #24699 ) ;
#23539 = ORIENTED_EDGE ( 'NONE', *, *, #16395, .T. ) ;
#23538 = ORIENTED_EDGE ( 'NONE', *, *, #11773, .F. ) ;
#23540 = CIRCLE ( 'NONE', #23093, 17.93072811908088937 ) ;
#23541 = EDGE_CURVE ( 'NONE', #21119, #15548, #27049, .T. ) ;
#23542 = CARTESIAN_POINT ( 'NONE',  ( 103.8044331943715122, 239.2408796537650346, -26.67200500018732612 ) ) ;
#23543 = ORIENTED_EDGE ( 'NONE', *, *, #9598, .F. ) ;
#23544 = VERTEX_POINT ( 'NONE', #16427 ) ;
#23545 = VERTEX_POINT ( 'NONE', #9954 ) ;
#23546 = ORIENTED_EDGE ( 'NONE', *, *, #8113, .T. ) ;
#23547 = ORIENTED_EDGE ( 'NONE', *, *, #24177, .T. ) ;
#23548 = VERTEX_POINT ( 'NONE', #23025 ) ;
#23549 = CIRCLE ( 'NONE', #11168, 6.204828372381208546 ) ;
#23550 = DIRECTION ( 'NONE',  ( 0.000000000000000000, 0.000000000000000000, -1.000000000000000000 ) ) ;
#23551 = VECTOR ( 'NONE', #20320, 1000.000000000000000 ) ;
#23552 = CARTESIAN_POINT ( 'NONE',  ( 158.0000000000014495, 66.01962454207041731, -45.00000000000000000 ) ) ;
#23553 = CIRCLE ( 'NONE', #11174, 22.49999999999999289 ) ;
#23554 = CARTESIAN_POINT ( 'NONE',  ( -196.7918453702777128, 20.24192588826928585, 80.00000000000001421 ) ) ;
#23555 = ADVANCED_FACE ( 'NONE', ( #23168 ), #1578, .F. ) ;
#23556 = CARTESIAN_POINT ( 'NONE',  ( 7.471928113118646131, 138.6332119385803594, -15.00000000000000178 ) ) ;
#23557 = EDGE_CURVE ( 'NONE', #14195, #9494, #3332, .T. ) ;
#23558 = LINE ( 'NONE', #25557, #14451 ) ;
#23559 = LINE ( 'NONE', #20972, #13673 ) ;
#23560 = DIRECTION ( 'NONE',  ( 0.8916010070298860946, -0.4528218681372321863, 0.000000000000000000 ) ) ;
#23561 = CARTESIAN_POINT ( 'NONE',  ( 111.5720349012335646, 201.2611006861219494, -148.9571385985325094 ) ) ;
#23562 = CARTESIAN_POINT ( 'NONE',  ( 158.0000000000014211, 73.03537455708450921, 45.00000000000000000 ) ) ;
#23563 = CARTESIAN_POINT ( 'NONE',  ( 157.4999999999997726, 248.8405625863305204, -45.00000000000000000 ) ) ;
#23564 = CARTESIAN_POINT ( 'NONE',  ( 0.000000000000000000, 0.000000000000000000, 100.0000000000000000 ) ) ;
#23565 = ORIENTED_EDGE ( 'NONE', *, *, #20762, .F. ) ;
#23566 = AXIS2_PLACEMENT_3D ( 'NONE', #11808, #20548, #9364 ) ;
#23567 = CARTESIAN_POINT ( 'NONE',  ( 117.2377723979416970, 233.8231604766229168, -99.61817846762012607 ) ) ;
#23568 = ADVANCED_FACE ( 'NONE', ( #18438 ), #27189, .F. ) ;
#23569 = VECTOR ( 'NONE', #26761, 1000.000000000000000 ) ;
#23570 = EDGE_CURVE ( 'NONE', #4881, #6807, #22783, .T. ) ;
#23571 = DIRECTION ( 'NONE',  ( 0.4528218681382319422, 0.8916010070293783896, -0.000000000000000000 ) ) ;
#23572 = VERTEX_POINT ( 'NONE', #21000 ) ;
#23573 = ITEM_DEFINED_TRANSFORMATION ( 'NONE', 'NONE', #16173,  #10637 ) ;
#23574 = EDGE_LOOP ( 'NONE', ( #15699, #2158 ) ) ;
#23575 = ORIENTED_EDGE ( 'NONE', *, *, #9389, .F. ) ;
#23576 = DIRECTION ( 'NONE',  ( 0.8916010070293384215, 0.4528218681383106015, 0.000000000000000000 ) ) ;
#23577 = PLANE ( 'NONE',  #2580 ) ;
#23578 = ORIENTED_EDGE ( 'NONE', *, *, #20344, .T. ) ;
#23580 = ADVANCED_FACE ( 'NONE', ( #1327 ), #10096, .F. ) ;
#23579 = ORIENTED_EDGE ( 'NONE', *, *, #17650, .T. ) ;
#23581 = LINE ( 'NONE', #11971, #8125 ) ;
#23582 = EDGE_CURVE ( 'NONE', #14705, #3225, #23444, .T. ) ;
#23583 = CARTESIAN_POINT ( 'NONE',  ( 103.3065434576170531, 238.5579404054215047, 26.03666308166562970 ) ) ;
#23584 = CARTESIAN_POINT ( 'NONE',  ( -192.2801638615682691, 101.7426455718185281, -32.00518413859087730 ) ) ;
#23585 = ORIENTED_EDGE ( 'NONE', *, *, #19310, .T. ) ;
#23586 = DIRECTION ( 'NONE',  ( 0.3102637045530707294, 0.9506505318133497973, 0.000000000000000000 ) ) ;
#23587 = ORIENTED_EDGE ( 'NONE', *, *, #13381, .F. ) ;
#23588 = AXIS2_PLACEMENT_3D ( 'NONE', #26334, #18157, #15441 ) ;
#23589 = CYLINDRICAL_SURFACE ( 'NONE', #2410, 5.000000000000004441 ) ;
#23590 = DIRECTION ( 'NONE',  ( -0.9659258262890670910, -0.2588190451025251804, 0.000000000000000000 ) ) ;
#23591 = VECTOR ( 'NONE', #2457, 1000.000000000000000 ) ;
#23592 = CARTESIAN_POINT ( 'NONE',  ( 134.9999999999998579, 433.5940952139197293, -145.0000000000000000 ) ) ;
#23593 = FACE_OUTER_BOUND ( 'NONE', #12855, .T. ) ;
#23594 = CARTESIAN_POINT ( 'NONE',  ( -194.9328835026024080, 99.53491429316976280, -32.53590786292448200 ) ) ;
#23595 = ORIENTED_EDGE ( 'NONE', *, *, #22761, .T. ) ;
#23596 = LINE ( 'NONE', #21432, #26052 ) ;
#23597 = CARTESIAN_POINT ( 'NONE',  ( 158.0000000000010516, 105.6377496546760568, 45.00000000000000000 ) ) ;
#23598 = CARTESIAN_POINT ( 'NONE',  ( 232.4749999999995964, 83.06687458711267880, -36.86484227207694175 ) ) ;
#23599 = DIRECTION ( 'NONE',  ( 0.000000000000000000, -1.000000000000000000, 0.000000000000000000 ) ) ;
#23600 = EDGE_LOOP ( 'NONE', ( #27626, #19509 ) ) ;
#23601 = DIRECTION ( 'NONE',  ( 0.4528218681370910770, -0.8916010070299578150, 0.000000000000000000 ) ) ;
#23602 = EDGE_CURVE ( 'NONE', #8797, #3340, #21286, .T. ) ;
#23603 = CARTESIAN_POINT ( 'NONE',  ( -203.1779787704217313, 93.05164332230201296, 28.77272332722132120 ) ) ;
#23604 = CARTESIAN_POINT ( 'NONE',  ( -214.3828916364065833, 175.2783111443768576, -13.00000000000000000 ) ) ;
#23605 = DIRECTION ( 'NONE',  ( 0.8916010070295106171, -0.4528218681379715393, 0.000000000000000000 ) ) ;
#23606 = VERTEX_POINT ( 'NONE', #12826 ) ;
#23607 = FACE_OUTER_BOUND ( 'NONE', #18216, .T. ) ;
#23608 = ORIENTED_EDGE ( 'NONE', *, *, #13669, .F. ) ;
#23609 = AXIS2_PLACEMENT_3D ( 'NONE', #22885, #12125, #14275 ) ;
#23610 = DIRECTION ( 'NONE',  ( -0.000000000000000000, -0.000000000000000000, 1.000000000000000000 ) ) ;
#23611 = CARTESIAN_POINT ( 'NONE',  ( -199.2320231536486403, 96.36337958803088100, -30.96155907179247890 ) ) ;
#23612 = VERTEX_POINT ( 'NONE', #14690 ) ;
#23613 = VECTOR ( 'NONE', #22371, 1000.000000000000114 ) ;
#23614 = VERTEX_POINT ( 'NONE', #26017 ) ;
#23615 = DIRECTION ( 'NONE',  ( 0.8916010070296940260, 0.4528218681376106058, 0.000000000000000000 ) ) ;
#23616 = VERTEX_POINT ( 'NONE', #8364 ) ;
#23617 = VERTEX_POINT ( 'NONE', #17260 ) ;
#23618 = ORIENTED_EDGE ( 'NONE', *, *, #18536, .F. ) ;
#23619 = ADVANCED_FACE ( 'NONE', ( #5778 ), #19132, .F. ) ;
#23620 = FACE_OUTER_BOUND ( 'NONE', #18006, .T. ) ;
#23621 = EDGE_CURVE ( 'NONE', #24673, #14597, #2956, .T. ) ;
#23622 = CARTESIAN_POINT ( 'NONE',  ( 158.0000000000016200, 52.97237449702815582, 45.00000000000000000 ) ) ;
#23623 = AXIS2_PLACEMENT_3D ( 'NONE', #16877, #5953, #12722 ) ;
#23624 = EDGE_CURVE ( 'NONE', #3986, #17824, #19935, .T. ) ;
#23625 = DIRECTION ( 'NONE',  ( 0.000000000000000000, 0.000000000000000000, -1.000000000000000000 ) ) ;
#23626 = CARTESIAN_POINT ( 'NONE',  ( -180.0000000000000284, -50.00000000000004263, 80.00000000000001421 ) ) ;
#23627 = VECTOR ( 'NONE', #13046, 999.9999999999998863 ) ;
#23628 = CIRCLE ( 'NONE', #15837, 41.00000000000000000 ) ;
#23629 = CARTESIAN_POINT ( 'NONE',  ( -279.3160071107327553, -512.7211954420570237, 0.000000000000000000 ) ) ;
#23630 = CYLINDRICAL_SURFACE ( 'NONE', #11269, 5.999999999999991118 ) ;
#23631 = CARTESIAN_POINT ( 'NONE',  ( -238.3574390336367514, 69.78222348740686698, -5.410870504202835995 ) ) ;
#23632 = ORIENTED_EDGE ( 'NONE', *, *, #16547, .T. ) ;
#23633 = DIRECTION ( 'NONE',  ( -0.8660254037844363761, 0.5000000000000041078, -0.000000000000000000 ) ) ;
#23634 = TOROIDAL_SURFACE ( 'NONE', #3442, 60.90601976618767566, 2.000000000000000000 ) ;
#23635 = CARTESIAN_POINT ( 'NONE',  ( 157.4999999999998579, 45.70268697826052318, -45.00000000000000000 ) ) ;
#23636 = LINE ( 'NONE', #26202, #21499 ) ;
#23637 = LINE ( 'NONE', #4369, #6144 ) ;
#23638 = EDGE_LOOP ( 'NONE', ( #8528, #16868, #18794, #23745 ) ) ;
#23639 = DIRECTION ( 'NONE',  ( 1.000000000000000000, -0.000000000000000000, -0.000000000000000000 ) ) ;
#23640 = DIRECTION ( 'NONE',  ( 0.000000000000000000, 0.000000000000000000, -1.000000000000000000 ) ) ;
#23641 = DIRECTION ( 'NONE',  ( 0.4528218681383106015, 0.8916010070293384215, -0.000000000000000000 ) ) ;
#23642 = CARTESIAN_POINT ( 'NONE',  ( -43.02437977270766112, 129.0347155322979233, 14.93735646117640847 ) ) ;
#23643 =( NAMED_UNIT ( * ) PLANE_ANGLE_UNIT ( ) SI_UNIT ( $, .RADIAN. ) );
#23644 = CARTESIAN_POINT ( 'NONE',  ( 79.99999999999995737, 59.99999999999998579, 45.00000000000000000 ) ) ;
#23645 = ORIENTED_EDGE ( 'NONE', *, *, #4876, .T. ) ;
#23646 = DIRECTION ( 'NONE',  ( 0.000000000000000000, -1.000000000000000000, 0.000000000000000000 ) ) ;
#23647 = ORIENTED_EDGE ( 'NONE', *, *, #27622, .T. ) ;
#23648 = CARTESIAN_POINT ( 'NONE',  ( 179.9999999999999147, -150.0000000000000284, 100.0000000000000142 ) ) ;
#23649 = ORIENTED_EDGE ( 'NONE', *, *, #6149, .T. ) ;
#23650 = CIRCLE ( 'NONE', #17675, 30.00000000000000000 ) ;
#23651 = VECTOR ( 'NONE', #25633, 1000.000000000000000 ) ;
#23652 = TOROIDAL_SURFACE ( 'NONE', #4361, 80.00000000000000000, 30.00000000000000000 ) ;
#23653 = ORIENTED_EDGE ( 'NONE', *, *, #24445, .T. ) ;
#23654 = CARTESIAN_POINT ( 'NONE',  ( -67.69391036949915019, 133.9331560312302258, 15.61747421727902463 ) ) ;
#23655 = VERTEX_POINT ( 'NONE', #12689 ) ;
#23656 = EDGE_CURVE ( 'NONE', #26678, #9167, #8926, .T. ) ;
#23657 = CIRCLE ( 'NONE', #7131, 4.999999999999997335 ) ;
#23658 = ORIENTED_EDGE ( 'NONE', *, *, #27823, .F. ) ;
#23659 = CARTESIAN_POINT ( 'NONE',  ( 157.4999999999998579, 146.0176872785422404, -45.00000000000000000 ) ) ;
#23660 = LINE ( 'NONE', #26084, #18776 ) ;
#23661 = LINE ( 'NONE', #19490, #6071 ) ;
#23662 = ADVANCED_FACE ( 'NONE', ( #23875 ), #12546, .F. ) ;
#23663 = ADVANCED_FACE ( 'NONE', ( #4180 ), #12149, .F. ) ;
#23664 = ADVANCED_FACE ( 'NONE', ( #6202 ), #16981, .T. ) ;
#23665 = CARTESIAN_POINT ( 'NONE',  ( -113.0279832246674232, 134.5396197302765700, -13.86330562916807274 ) ) ;
#23666 = CARTESIAN_POINT ( 'NONE',  ( -270.4051725677463764, -170.3149295705450186, -88.16521414542363289 ) ) ;
#23667 = CARTESIAN_POINT ( 'NONE',  ( -261.2691008037259053, -166.7184843738689608, 90.00000000000001421 ) ) ;
#23668 = CARTESIAN_POINT ( 'NONE',  ( -214.9809428154103728, 87.87766106360727747, -21.23882047124828176 ) ) ;
#23669 = PLANE ( 'NONE',  #19554 ) ;
#23670 = VECTOR ( 'NONE', #3331, 1000.000000000000000 ) ;
#23671 = CARTESIAN_POINT ( 'NONE',  ( -203.2481855153402250, 92.57460631283319685, 29.78692811926998729 ) ) ;
#23672 = DIRECTION ( 'NONE',  ( 0.9784193629480828491, 0.2066290158914464437, 0.000000000000000000 ) ) ;
#23673 = CARTESIAN_POINT ( 'NONE',  ( 157.9999999999998295, 231.0315000300280417, 45.00000000000000000 ) ) ;
#23674 = DIRECTION ( 'NONE',  ( 0.8916010070293383105, -0.4528218681383106015, 0.000000000000000000 ) ) ;
#23675 = VECTOR ( 'NONE', #16590, 1000.000000000000000 ) ;
#23676 = ORIENTED_EDGE ( 'NONE', *, *, #27528, .F. ) ;
#23677 = CARTESIAN_POINT ( 'NONE',  ( 157.9999999999997726, 248.5866250825770294, -45.00000000000000000 ) ) ;
#23678 = CARTESIAN_POINT ( 'NONE',  ( 157.9999999999997158, 261.6338751276190351, 45.00000000000000000 ) ) ;
#23679 = LINE ( 'NONE', #21516, #1440 ) ;
#23680 = VECTOR ( 'NONE', #17506, 1000.000000000000000 ) ;
#23682 = ORIENTED_EDGE ( 'NONE', *, *, #23878, .T. ) ;
#23681 = ORIENTED_EDGE ( 'NONE', *, *, #23621, .T. ) ;
#23683 = CARTESIAN_POINT ( 'NONE',  ( 96.29556199549620032, 241.0127520899152387, -10.03785181564776963 ) ) ;
#23684 = VERTEX_POINT ( 'NONE', #2030 ) ;
#23685 = ORIENTED_EDGE ( 'NONE', *, *, #22919, .T. ) ;
#23686 = ORIENTED_EDGE ( 'NONE', *, *, #15186, .F. ) ;
#23687 = ADVANCED_FACE ( 'NONE', ( #19562 ), #28020, .F. ) ;
#23688 = EDGE_CURVE ( 'NONE', #19409, #18723, #3612, .T. ) ;
#23689 = ORIENTED_EDGE ( 'NONE', *, *, #24971, .F. ) ;
#23690 = VERTEX_POINT ( 'NONE', #16843 ) ;
#23691 = ORIENTED_EDGE ( 'NONE', *, *, #12830, .F. ) ;
#23692 = CIRCLE ( 'NONE', #27811, 22.49999999999999289 ) ;
#23693 = CARTESIAN_POINT ( 'NONE',  ( 158.0000000000000284, 203.9527499549551806, 45.00000000000000000 ) ) ;
#23694 = ADVANCED_FACE ( 'NONE', ( #14839 ), #1467, .T. ) ;
#23695 = ADVANCED_FACE ( 'NONE', ( #3756 ), #1606, .F. ) ;
#23696 = CARTESIAN_POINT ( 'NONE',  ( 65.00000000000000000, -120.0000000000000711, 70.00000000000001421 ) ) ;
#23697 = AXIS2_PLACEMENT_3D ( 'NONE', #24369, #17907, #13613 ) ;
#23698 = DIRECTION ( 'NONE',  ( -0.8916010070296226386, -0.4528218681377511046, 0.000000000000000000 ) ) ;
#23699 = LINE ( 'NONE', #15374, #25261 ) ;
#23700 = DIRECTION ( 'NONE',  ( -0.000000000000000000, 1.000000000000000000, 0.000000000000000000 ) ) ;
#23701 = FACE_OUTER_BOUND ( 'NONE', #2754, .T. ) ;
#23702 = CARTESIAN_POINT ( 'NONE',  ( -227.7405116417571946, 73.49447507798586798, -17.05698111974955111 ) ) ;
#23703 = CARTESIAN_POINT ( 'NONE',  ( -42.53273978471831640, 130.9733465240572627, 14.93735646117640670 ) ) ;
#23704 = DIRECTION ( 'NONE',  ( -0.000000000000000000, 0.000000000000000000, -1.000000000000000000 ) ) ;
#23705 = DIRECTION ( 'NONE',  ( -3.053113317719176147E-15, -4.035281788239917819E-31, -1.000000000000000000 ) ) ;
#23706 = CARTESIAN_POINT ( 'NONE',  ( 158.0000000000007958, 130.7164997297464595, -45.00000000000000000 ) ) ;
#23707 = EDGE_LOOP ( 'NONE', ( #5698, #4169, #19574, #20328 ) ) ;
#23708 = VECTOR ( 'NONE', #3928, 999.9999999999998863 ) ;
#23709 = CARTESIAN_POINT ( 'NONE',  ( -186.0983758910577990, 106.1011689576974248, 31.60744335178514319 ) ) ;
#23710 = CARTESIAN_POINT ( 'NONE',  ( 217.4999999999996305, 258.6181251126050711, 6.000000000000019540 ) ) ;
#23711 = VERTEX_POINT ( 'NONE', #3900 ) ;
#23712 = ADVANCED_FACE ( 'NONE', ( #21428 ), #2028, .F. ) ;
#23713 = ORIENTED_EDGE ( 'NONE', *, *, #8845, .F. ) ;
#23714 = VERTEX_POINT ( 'NONE', #6484 ) ;
#23715 = ADVANCED_FACE ( 'NONE', ( #4325 ), #8783, .F. ) ;
#23716 = CARTESIAN_POINT ( 'NONE',  ( 113.4920585194047078, 104.4775165427241319, 100.0000000000000142 ) ) ;
#23717 = CARTESIAN_POINT ( 'NONE',  ( 110.9201389036588949, 220.0000000000000284, 153.1081322850112940 ) ) ;
#23718 = EDGE_LOOP ( 'NONE', ( #25415, #16906, #26885, #28174 ) ) ;
#23719 = ORIENTED_EDGE ( 'NONE', *, *, #1466, .F. ) ;
#23720 = CARTESIAN_POINT ( 'NONE',  ( 101.7779539750033280, 119.2876405404464890, -82.50000000032424907 ) ) ;
#23721 = CARTESIAN_POINT ( 'NONE',  ( 99.01626835887864786, 234.2217840360999332, 21.79255213936348312 ) ) ;
#23722 = DIRECTION ( 'NONE',  ( 1.000000000000000000, 2.312964634635742957E-16, 0.000000000000000000 ) ) ;
#23723 = ORIENTED_EDGE ( 'NONE', *, *, #13572, .T. ) ;
#23724 = CARTESIAN_POINT ( 'NONE',  ( -206.8923702502391393, 90.46133927671940000, 26.11705481793761052 ) ) ;
#23725 = ORIENTED_EDGE ( 'NONE', *, *, #11868, .F. ) ;
#23726 = VECTOR ( 'NONE', #12228, 1000.000000000000000 ) ;
#23727 = DIRECTION ( 'NONE',  ( 0.000000000000000000, 0.000000000000000000, -1.000000000000000000 ) ) ;
#23728 = AXIS2_PLACEMENT_3D ( 'NONE', #4422, #17495, #13347 ) ;
#23729 = EDGE_CURVE ( 'NONE', #1362, #21744, #8928, .T. ) ;
#23730 = DIRECTION ( 'NONE',  ( 0.000000000000000000, 0.000000000000000000, -1.000000000000000000 ) ) ;
#23731 = DIRECTION ( 'NONE',  ( 1.000000000000000000, 4.533410683886055032E-14, 0.000000000000000000 ) ) ;
#23732 = DIRECTION ( 'NONE',  ( 1.000000000000000000, -0.000000000000000000, -0.000000000000000000 ) ) ;
#23733 = VERTEX_POINT ( 'NONE', #10945 ) ;
#23734 = LINE ( 'NONE', #4187, #6795 ) ;
#23735 = FACE_OUTER_BOUND ( 'NONE', #10793, .T. ) ;
#23736 = DIRECTION ( 'NONE',  ( 0.000000000000000000, 0.000000000000000000, -1.000000000000000000 ) ) ;
#23737 = CARTESIAN_POINT ( 'NONE',  ( 204.8742559748123426, 133.4291290931197977, 45.00000000000000000 ) ) ;
#23738 = ORIENTED_EDGE ( 'NONE', *, *, #20597, .F. ) ;
#23739 = EDGE_CURVE ( 'NONE', #9830, #25647, #15840, .T. ) ;
#23740 = CARTESIAN_POINT ( 'NONE',  ( 179.9999999999999147, 0.000000000000000000, 100.0000000000000142 ) ) ;
#23741 = AXIS2_PLACEMENT_3D ( 'NONE', #5918, #14416, #23308 ) ;
#23742 = CARTESIAN_POINT ( 'NONE',  ( -184.3234090630027140, 107.2774685039649114, 31.16804357237790057 ) ) ;
#23743 = CARTESIAN_POINT ( 'NONE',  ( 33.10302365956999182, 203.2034914284457159, -13.00000000000000000 ) ) ;
#23744 = CARTESIAN_POINT ( 'NONE',  ( -219.0825447683637606, 87.83772393549990909, 16.88515830131742490 ) ) ;
#23745 = ORIENTED_EDGE ( 'NONE', *, *, #19364, .F. ) ;
#23746 = SHAPE_REPRESENTATION_RELATIONSHIP ( 'NONE' , 'NONE' ,  #24038, #19102 ) ;
#23747 = DIRECTION ( 'NONE',  ( -0.000000000000000000, -0.000000000000000000, -1.000000000000000000 ) ) ;
#23748 = ORIENTED_EDGE ( 'NONE', *, *, #3666, .T. ) ;
#23749 = TOROIDAL_SURFACE ( 'NONE', #27405, 55.86582179324592090, 2.000000000000000000 ) ;
#23750 = EDGE_CURVE ( 'NONE', #2290, #2948, #11380, .T. ) ;
#23751 = DIRECTION ( 'NONE',  ( -0.000000000000000000, -0.000000000000000000, -1.000000000000000000 ) ) ;
#23752 = CARTESIAN_POINT ( 'NONE',  ( -168.1616170882788026, 116.6881954979569258, -24.56124631037856076 ) ) ;
#23753 = ORIENTED_EDGE ( 'NONE', *, *, #8470, .F. ) ;
#23754 = ORIENTED_EDGE ( 'NONE', *, *, #22268, .F. ) ;
#23755 = DIRECTION ( 'NONE',  ( 0.4528218681383003319, 0.8916010070293436396, 0.000000000000000000 ) ) ;
#23756 = ORIENTED_EDGE ( 'NONE', *, *, #27072, .F. ) ;
#23757 = VERTEX_POINT ( 'NONE', #17688 ) ;
#23758 = ORIENTED_EDGE ( 'NONE', *, *, #17759, .F. ) ;
#23759 = CARTESIAN_POINT ( 'NONE',  ( 158.0000000000009948, 110.6534996696901345, -45.00000000000000000 ) ) ;
#23760 = ADVANCED_FACE ( 'NONE', ( #13116 ), #26436, .F. ) ;
#23761 = CIRCLE ( 'NONE', #8161, 166.0121251338587172 ) ;
#23762 = EDGE_CURVE ( 'NONE', #17397, #23714, #17640, .T. ) ;
#23763 = CARTESIAN_POINT ( 'NONE',  ( 33.10302365956999182, 219.6666220619077876, -15.00000000000000000 ) ) ;
#23764 = CYLINDRICAL_SURFACE ( 'NONE', #24968, 5.999999999999977796 ) ;
#23765 = LINE ( 'NONE', #4076, #20906 ) ;
#23766 = CARTESIAN_POINT ( 'NONE',  ( 232.4999999999996305, 194.4107529906318064, -62.90796922943941638 ) ) ;
#23767 = DIRECTION ( 'NONE',  ( 1.000000000000000000, 0.000000000000000000, 0.000000000000000000 ) ) ;
#23768 = CARTESIAN_POINT ( 'NONE',  ( -228.3003245610471481, 63.46411924055758647, -17.58993856061233529 ) ) ;
#23769 = ORIENTED_EDGE ( 'NONE', *, *, #15337, .T. ) ;
#23770 =( REPRESENTATION_RELATIONSHIP ('NONE','NONE', #11963, #201 ) REPRESENTATION_RELATIONSHIP_WITH_TRANSFORMATION ( #23573 )SHAPE_REPRESENTATION_RELATIONSHIP( ) );
#23771 = DIRECTION ( 'NONE',  ( 1.000000000000000000, 0.000000000000000000, 0.000000000000000000 ) ) ;
#23772 = PLANE ( 'NONE',  #1007 ) ;
#23773 = DIRECTION ( 'NONE',  ( 0.000000000000000000, 0.000000000000000000, -1.000000000000000000 ) ) ;
#23774 = LINE ( 'NONE', #15169, #15328 ) ;
#23775 = VERTEX_POINT ( 'NONE', #17541 ) ;
#23776 = EDGE_CURVE ( 'NONE', #4884, #13140, #21861, .T. ) ;
#23777 = DIRECTION ( 'NONE',  ( -0.8916010070297749612, -0.4528218681374510668, 0.000000000000000000 ) ) ;
#23778 = VECTOR ( 'NONE', #12600, 1000.000000000000000 ) ;
#23779 = DIRECTION ( 'NONE',  ( 1.000000000000000000, 0.000000000000000000, 0.000000000000000000 ) ) ;
#23780 = CARTESIAN_POINT ( 'NONE',  ( -272.4384950037861017, -165.0368469557824085, 87.33088399392040913 ) ) ;
#23781 = DIRECTION ( 'NONE',  ( -0.8916010070293384215, 0.4528218681383106015, 0.000000000000000000 ) ) ;
#23782 = DIRECTION ( 'NONE',  ( -0.8916010070294402290, -0.4528218681381102062, 0.000000000000000000 ) ) ;
#23783 = DIRECTION ( 'NONE',  ( 0.9659258262890670910, -0.2588190451025251804, 0.000000000000000000 ) ) ;
#23784 = VERTEX_POINT ( 'NONE', #4603 ) ;
#23785 = EDGE_CURVE ( 'NONE', #7159, #15242, #2167, .T. ) ;
#23786 = ADVANCED_FACE ( 'NONE', ( #4460 ), #4891, .F. ) ;
#23787 = AXIS2_PLACEMENT_3D ( 'NONE', #5820, #25366, #18756 ) ;
#23788 = DIRECTION ( 'NONE',  ( -0.8660254037844363761, 0.5000000000000039968, -0.000000000000000000 ) ) ;
#23789 = VERTEX_POINT ( 'NONE', #24161 ) ;
#23790 = DIRECTION ( 'NONE',  ( 0.4528218681383106015, -0.8916010070293384215, 0.000000000000000000 ) ) ;
#23791 = VECTOR ( 'NONE', #4360, 1000.000000000000000 ) ;
#23792 = ORIENTED_EDGE ( 'NONE', *, *, #14485, .T. ) ;
#23793 = EDGE_CURVE ( 'NONE', #1877, #11276, #21308, .T. ) ;
#23794 = ORIENTED_EDGE ( 'NONE', *, *, #1428, .F. ) ;
#23795 = DIRECTION ( 'NONE',  ( 1.000000000000000000, 0.000000000000000000, -0.000000000000000000 ) ) ;
#23796 = ORIENTED_EDGE ( 'NONE', *, *, #23944, .F. ) ;
#23797 = ORIENTED_EDGE ( 'NONE', *, *, #20283, .F. ) ;
#23798 = VERTEX_POINT ( 'NONE', #21996 ) ;
#23799 = CARTESIAN_POINT ( 'NONE',  ( -217.7401460507702780, 138.5677444271782122, 12.99353264123212703 ) ) ;
#23800 = CARTESIAN_POINT ( 'NONE',  ( -127.2321417042300311, 130.3961964139149075, -16.54948570837689914 ) ) ;
#23801 = CARTESIAN_POINT ( 'NONE',  ( -211.9382648910248577, -218.8137564101509724, 92.60662834576568514 ) ) ;
#23802 = VECTOR ( 'NONE', #2713, 1000.000000000000000 ) ;
#23803 = CARTESIAN_POINT ( 'NONE',  ( -158.3239166661295485, 121.3790681822268738, -21.42498206582862608 ) ) ;
#23804 = EDGE_CURVE ( 'NONE', #3911, #16524, #2303, .T. ) ;
#23805 = PLANE ( 'NONE',  #18811 ) ;
#23806 = DIRECTION ( 'NONE',  ( 0.000000000000000000, -1.000000000000000000, 0.000000000000000000 ) ) ;
#23807 = AXIS2_PLACEMENT_3D ( 'NONE', #25430, #3584, #8334 ) ;
#23808 = DIRECTION ( 'NONE',  ( -0.7059982162894324897, 0.7082136108520787898, 0.000000000000000000 ) ) ;
#23809 = CARTESIAN_POINT ( 'NONE',  ( -220.6589170087162017, 88.04539541979674766, -18.04441532903050671 ) ) ;
#23810 = PRODUCT_DEFINITION_SHAPE ( 'NONE', 'NONE',  #28406 ) ;
#23811 = CARTESIAN_POINT ( 'NONE',  ( 132.5217165206440200, 249.8980084815856912, -139.5322470298331439 ) ) ;
#23812 = VECTOR ( 'NONE', #7058, 1000.000000000000000 ) ;
#23813 = LINE ( 'NONE', #6843, #4837 ) ;
#23814 = FACE_OUTER_BOUND ( 'NONE', #25291, .T. ) ;
#23815 = DIRECTION ( 'NONE',  ( 0.000000000000000000, 0.000000000000000000, -1.000000000000000000 ) ) ;
#23816 = CARTESIAN_POINT ( 'NONE',  ( 157.4999999999998579, 85.82868709837320864, 45.00000000000000000 ) ) ;
#23817 = VERTEX_POINT ( 'NONE', #17828 ) ;
#23818 = CARTESIAN_POINT ( 'NONE',  ( 119.9999999999999147, 140.0000000000000000, 100.0000000000000142 ) ) ;
#23819 = CARTESIAN_POINT ( 'NONE',  ( 158.0000000000012221, 90.59049960963380954, 45.00000000000000000 ) ) ;
#23820 = DIRECTION ( 'NONE',  ( -0.8916010070296023216, -0.4528218681377911281, 0.000000000000000000 ) ) ;
#23821 = EDGE_LOOP ( 'NONE', ( #28222, #6546, #14217, #10153 ) ) ;
#23822 = EDGE_CURVE ( 'NONE', #13520, #26295, #25427, .T. ) ;
#23823 = EDGE_CURVE ( 'NONE', #27477, #15024, #672, .T. ) ;
#23824 = AXIS2_PLACEMENT_3D ( 'NONE', #16023, #27202, #9261 ) ;
#23825 = CARTESIAN_POINT ( 'NONE',  ( 105.2802062291979581, 246.7841820210335584, -28.66020632211111518 ) ) ;
#23826 = VERTEX_POINT ( 'NONE', #11232 ) ;
#23827 = CARTESIAN_POINT ( 'NONE',  ( -4.329483062107786218, 134.1423878703578225, -13.93341408620584687 ) ) ;
#23828 = ORIENTED_EDGE ( 'NONE', *, *, #14170, .T. ) ;
#23829 = AXIS2_PLACEMENT_3D ( 'NONE', #2592, #15836, #4889 ) ;
#23830 = VERTEX_POINT ( 'NONE', #19983 ) ;
#23831 = VECTOR ( 'NONE', #19220, 1000.000000000000000 ) ;
#23832 = VERTEX_POINT ( 'NONE', #9216 ) ;
#23833 = VERTEX_POINT ( 'NONE', #26582 ) ;
#23834 = ORIENTED_EDGE ( 'NONE', *, *, #7062, .F. ) ;
#23835 = LINE ( 'NONE', #10764, #6761 ) ;
#23836 = CIRCLE ( 'NONE', #18784, 53.86582179324592090 ) ;
#23837 = EDGE_CURVE ( 'NONE', #1313, #16168, #6910, .T. ) ;
#23838 = PLANE ( 'NONE',  #16061 ) ;
#23839 = PRODUCT_DEFINITION_CONTEXT ( 'detailed design', #2664, 'design' ) ;
#23840 = DIRECTION ( 'NONE',  ( 0.8916010070299774659, -0.4528218681370523302, 0.000000000000000000 ) ) ;
#23841 = DIRECTION ( 'NONE',  ( -0.8916010070294903000, 0.4528218681380115629, 0.000000000000000000 ) ) ;
#23842 = VECTOR ( 'NONE', #5334, 999.9999999999998863 ) ;
#23843 = EDGE_CURVE ( 'NONE', #13590, #27375, #22285, .T. ) ;
#23844 = LINE ( 'NONE', #12235, #1150 ) ;
#23845 = CARTESIAN_POINT ( 'NONE',  ( 158.0000000000009379, 118.1771246922112653, 45.00000000000000000 ) ) ;
#23846 = FACE_OUTER_BOUND ( 'NONE', #18464, .T. ) ;
#23847 = CIRCLE ( 'NONE', #18801, 5.000000000000000888 ) ;
#23848 = DIRECTION ( 'NONE',  ( -0.8916010070295208312, 0.4528218681379515553, 0.000000000000000000 ) ) ;
#23849 = CARTESIAN_POINT ( 'NONE',  ( -210.0000000000000568, 59.99999999999992895, 18.66498670256683212 ) ) ;
#23850 = LINE ( 'NONE', #12517, #2335 ) ;
#23851 = ADVANCED_FACE ( 'NONE', ( #11676 ), #27155, .T. ) ;
#23852 = DIRECTION ( 'NONE',  ( 0.000000000000000000, 0.000000000000000000, 1.000000000000000000 ) ) ;
#23853 = VERTEX_POINT ( 'NONE', #27424 ) ;
#23854 = DIRECTION ( 'NONE',  ( -0.000000000000000000, 1.000000000000000000, -0.000000000000000000 ) ) ;
#23855 = EDGE_CURVE ( 'NONE', #17304, #25380, #18123, .T. ) ;
#23856 = EDGE_CURVE ( 'NONE', #27854, #11176, #15979, .T. ) ;
#23857 = CARTESIAN_POINT ( 'NONE',  ( -277.2150368962633706, -170.0000000000001137, -101.5769467933888279 ) ) ;
#23858 = EDGE_LOOP ( 'NONE', ( #15907, #16455, #6327, #16356 ) ) ;
#23859 = CONTEXT_DEPENDENT_SHAPE_REPRESENTATION ( #25604, #16684 ) ;
#23860 = ORIENTED_EDGE ( 'NONE', *, *, #20073, .F. ) ;
#23861 = ORIENTED_EDGE ( 'NONE', *, *, #2826, .F. ) ;
#23862 = CARTESIAN_POINT ( 'NONE',  ( 157.4999999999996589, 281.4429376839215138, 45.00000000000000000 ) ) ;
#23863 = VECTOR ( 'NONE', #18611, 1000.000000000000000 ) ;
#23864 = DIRECTION ( 'NONE',  ( 0.8916010070296838119, 0.4528218681376304788, 0.000000000000000000 ) ) ;
#23865 = ORIENTED_EDGE ( 'NONE', *, *, #18979, .F. ) ;
#23866 = EDGE_LOOP ( 'NONE', ( #20777, #1636 ) ) ;
#23867 = CARTESIAN_POINT ( 'NONE',  ( 319.9779125536060178, 113.2029523930392969, -145.0000000000000000 ) ) ;
#23868 = AXIS2_PLACEMENT_3D ( 'NONE', #3577, #21252, #14379 ) ;
#23869 = DIRECTION ( 'NONE',  ( 0.000000000000000000, -0.3247168404252948615, -0.9458112779747414045 ) ) ;
#23870 = CARTESIAN_POINT ( 'NONE',  ( 158.0000000000009663, 113.6692496847042264, 45.00000000000000000 ) ) ;
#23871 = ORIENTED_EDGE ( 'NONE', *, *, #7857, .T. ) ;
#23872 = CARTESIAN_POINT ( 'NONE',  ( -225.7040669049297037, 89.49289086750439992, 16.08021328254498883 ) ) ;
#23873 = ORIENTED_EDGE ( 'NONE', *, *, #25693, .T. ) ;
#23874 = CARTESIAN_POINT ( 'NONE',  ( 65.00000000000000000, -120.0000000000000995, -69.99999999999998579 ) ) ;
#23875 = FACE_OUTER_BOUND ( 'NONE', #8168, .T. ) ;
#23876 = CARTESIAN_POINT ( 'NONE',  ( 0.000000000000000000, 0.000000000000000000, 110.0000000000000284 ) ) ;
#23877 = DIRECTION ( 'NONE',  ( 0.4528218681380314914, 0.8916010070294801970, -0.000000000000000000 ) ) ;
#23878 = EDGE_CURVE ( 'NONE', #26636, #23123, #17212, .T. ) ;
#23879 = ORIENTED_EDGE ( 'NONE', *, *, #19086, .F. ) ;
#23880 = VECTOR ( 'NONE', #13012, 1000.000000000000000 ) ;
#23881 = CARTESIAN_POINT ( 'NONE',  ( 115.6411010564578561, 208.5333949360010308, 99.00000000000001421 ) ) ;
#23882 = DIRECTION ( 'NONE',  ( 1.000000000000000000, -0.000000000000000000, -0.000000000000000000 ) ) ;
#23883 = DIRECTION ( 'NONE',  ( -0.000000000000000000, 0.000000000000000000, 1.000000000000000000 ) ) ;
#23884 = CARTESIAN_POINT ( 'NONE',  ( -277.2150368962633706, -170.0000000000001137, -101.5769467933888137 ) ) ;
#23885 = ORIENTED_EDGE ( 'NONE', *, *, #18926, .T. ) ;
#23886 = FACE_BOUND ( 'NONE', #1164, .T. ) ;
#23887 = VECTOR ( 'NONE', #21960, 1000.000000000000000 ) ;
#23888 = EDGE_CURVE ( 'NONE', #15403, #13270, #5184, .T. ) ;
#23889 = CARTESIAN_POINT ( 'NONE',  ( -175.4043012490592730, 112.7503553874411608, 27.84382049740324305 ) ) ;
#23890 = CARTESIAN_POINT ( 'NONE',  ( -235.6837214056122036, 120.7228219557777180, 12.99999999999999822 ) ) ;
#23891 = CARTESIAN_POINT ( 'NONE',  ( -223.0800714857218452, 88.58381330274964682, 14.94850374233409696 ) ) ;
#23892 = ORIENTED_EDGE ( 'NONE', *, *, #23888, .F. ) ;
#23893 = LINE ( 'NONE', #26999, #9770 ) ;
#23894 = VERTEX_POINT ( 'NONE', #11809 ) ;
#23895 = ADVANCED_FACE ( 'NONE', ( #14244 ), #13552, .T. ) ;
#23896 = CARTESIAN_POINT ( 'NONE',  ( -260.0000000000001137, -220.0000000000000853, -109.9999999999998721 ) ) ;
#23897 = CARTESIAN_POINT ( 'NONE',  ( -164.2202815706227454, 118.6546980540646956, -23.76065989308352755 ) ) ;
#23898 = ORIENTED_EDGE ( 'NONE', *, *, #7344, .T. ) ;
#23899 = ORIENTED_EDGE ( 'NONE', *, *, #9093, .F. ) ;
#23900 = CARTESIAN_POINT ( 'NONE',  ( 354.3612859273441700, 105.7287271543778076, -145.0000000000000000 ) ) ;
#23901 = ORIENTED_EDGE ( 'NONE', *, *, #13917, .T. ) ;
#23902 = VECTOR ( 'NONE', #7386, 1000.000000000000000 ) ;
#23903 = DIRECTION ( 'NONE',  ( 0.4528218681377710886, -0.8916010070296124246, 0.000000000000000000 ) ) ;
#23904 = ORIENTED_EDGE ( 'NONE', *, *, #16045, .F. ) ;
#23905 = VERTEX_POINT ( 'NONE', #3441 ) ;
#23906 = DIRECTION ( 'NONE',  ( 0.000000000000000000, -1.000000000000000000, 0.000000000000000000 ) ) ;
#23907 = VECTOR ( 'NONE', #18269, 1000.000000000000114 ) ;
#23908 = CARTESIAN_POINT ( 'NONE',  ( 164.9999999999998579, 220.0000000000000284, -122.9999999999999574 ) ) ;
#23909 = CARTESIAN_POINT ( 'NONE',  ( -5.421010862427522170E-17, 1.249999999999999778, 7.098227728112298962 ) ) ;
#23910 = DIRECTION ( 'NONE',  ( -0.000000000000000000, -0.000000000000000000, -1.000000000000000000 ) ) ;
#23911 = LINE ( 'NONE', #10983, #23880 ) ;
#23912 = DIRECTION ( 'NONE',  ( 0.000000000000000000, -1.000000000000000000, 0.000000000000000000 ) ) ;
#23913 = ADVANCED_FACE ( 'NONE', ( #13826 ), #3158, .F. ) ;
#23914 = CARTESIAN_POINT ( 'NONE',  ( -235.2766700735766960, 67.45978041261076896, -15.24953891110926918 ) ) ;
#23915 = ORIENTED_EDGE ( 'NONE', *, *, #26187, .T. ) ;
#23916 = DIRECTION ( 'NONE',  ( 0.4528218681377511601, -0.8916010070296226386, 0.000000000000000000 ) ) ;
#23917 = B_SPLINE_CURVE_WITH_KNOTS ( 'NONE', 3,
 ( #23881, #2035, #10809, #28306, #17408, #26167, #17546, #13119 ),
 .UNSPECIFIED., .F., .F.,
 ( 4, 2, 2, 4 ),
 ( 0.03156115556266906458, 0.03330631506936755637, 0.03505147457606604816, 0.03854179358946308726 ),
 .UNSPECIFIED. ) ;
#23918 = DIRECTION ( 'NONE',  ( -0.000000000000000000, 1.214306433183764720E-16, -1.000000000000000000 ) ) ;
#23919 = DIRECTION ( 'NONE',  ( 0.000000000000000000, 0.000000000000000000, -1.000000000000000000 ) ) ;
#23920 = LINE ( 'NONE', #10710, #26774 ) ;
#23921 = ORIENTED_EDGE ( 'NONE', *, *, #8250, .T. ) ;
#23922 = PLANE ( 'NONE',  #22447 ) ;
#23923 = AXIS2_PLACEMENT_3D ( 'NONE', #9759, #27264, #8588 ) ;
#23924 = CARTESIAN_POINT ( 'NONE',  ( 157.6866818850739662, 8.471341669691319964, 45.00000000000000000 ) ) ;
#23925 = DIRECTION ( 'NONE',  ( -0.8916010070294700940, 0.4528218681380514754, 0.000000000000000000 ) ) ;
#23926 = CARTESIAN_POINT ( 'NONE',  ( 157.4999999999997158, 263.8878126313725829, 45.00000000000000000 ) ) ;
#23927 = CARTESIAN_POINT ( 'NONE',  ( 187.4999999999996305, 288.9665627064425166, -45.00000000000000000 ) ) ;
#23928 = ORIENTED_EDGE ( 'NONE', *, *, #6104, .F. ) ;
#23929 = VECTOR ( 'NONE', #21479, 1000.000000000000114 ) ;
#23930 = CIRCLE ( 'NONE', #24396, 5.999999999999991118 ) ;
#23931 = EDGE_CURVE ( 'NONE', #13241, #27691, #12090, .T. ) ;
#23932 = CARTESIAN_POINT ( 'NONE',  ( 134.9999999999998579, 220.0000000000000284, -90.00000000000002842 ) ) ;
#23933 = VERTEX_POINT ( 'NONE', #25283 ) ;
#23934 = ADVANCED_FACE ( 'NONE', ( #5038, #9646 ), #5604, .F. ) ;
#23935 = CARTESIAN_POINT ( 'NONE',  ( -261.1919288306253293, -171.9377729149742038, 95.00000000000004263 ) ) ;
#23936 = ORIENTED_EDGE ( 'NONE', *, *, #13349, .T. ) ;
#23937 = ORIENTED_EDGE ( 'NONE', *, *, #14019, .T. ) ;
#23938 = CARTESIAN_POINT ( 'NONE',  ( 157.4999999999998579, 130.9704372334999789, -45.00000000000000000 ) ) ;
#23939 = ORIENTED_EDGE ( 'NONE', *, *, #2482, .F. ) ;
#23940 = ORIENTED_EDGE ( 'NONE', *, *, #11340, .T. ) ;
#23941 = EDGE_CURVE ( 'NONE', #18196, #17639, #20687, .T. ) ;
#23942 = CARTESIAN_POINT ( 'NONE',  ( -92.57281119172596107, 134.7193011466158339, -15.46818772961191257 ) ) ;
#23943 = CARTESIAN_POINT ( 'NONE',  ( -213.0248109774373688, -217.2055523511229467, 94.52687028321123819 ) ) ;
#23944 = EDGE_CURVE ( 'NONE', #16156, #13878, #16119, .T. ) ;
#23945 = AXIS2_PLACEMENT_3D ( 'NONE', #16988, #3908, #21297 ) ;
#23946 = CARTESIAN_POINT ( 'NONE',  ( 158.0000000000002558, 181.3818748873943889, -45.00000000000000000 ) ) ;
#23947 = B_SPLINE_CURVE_WITH_KNOTS ( 'NONE', 3,
 ( #13342, #17349, #15641, #15215, #26256, #23827, #11038, #19787, #4135, #23969, #10897, #11180, #19652, #22233, #28389, #26388, #115, #2396, #11329, #17924, #6717, #28259, #8737, #12918 ),
 .UNSPECIFIED., .F., .F.,
 ( 4, 2, 2, 2, 2, 2, 2, 2, 2, 2, 2, 4 ),
 ( 0.000000000000000000, 0.006705505486134448294, 0.01341101097226889659, 0.01676376371533612117, 0.02011651645840334748, 0.02682202194453779318, 0.03352752743067224928, 0.03520390380220585202, 0.03688028017373946171, 0.04023303291680666027, 0.04693853840294105045, 0.05364404388907543370 ),
 .UNSPECIFIED. ) ;
#23948 = CARTESIAN_POINT ( 'NONE',  ( -189.8086322075389774, 92.49158130768422836, 12.99999999999999822 ) ) ;
#23949 = VECTOR ( 'NONE', #8947, 1000.000000000000227 ) ;
#23950 = VECTOR ( 'NONE', #16030, 1000.000000000000000 ) ;
#23951 = LINE ( 'NONE', #13462, #27983 ) ;
#23952 = CARTESIAN_POINT ( 'NONE',  ( -274.7557459110828972, -170.0000000000001421, 86.12025961983464128 ) ) ;
#23953 = LINE ( 'NONE', #57, #19533 ) ;
#23954 = DIRECTION ( 'NONE',  ( -0.000000000000000000, -0.000000000000000000, -1.000000000000000000 ) ) ;
#23955 = DIRECTION ( 'NONE',  ( 0.8660254037844432595, 0.4999999999999919509, -0.000000000000000000 ) ) ;
#23956 = EDGE_CURVE ( 'NONE', #25233, #2802, #13971, .T. ) ;
#23957 = DIRECTION ( 'NONE',  ( -0.000000000000000000, 0.000000000000000000, 1.000000000000000000 ) ) ;
#23958 = CARTESIAN_POINT ( 'NONE',  ( 158.0000000000004832, 161.3188748273380213, 45.00000000000000000 ) ) ;
#23959 = DIRECTION ( 'NONE',  ( -1.000000000000000000, -4.625929269271485914E-16, 0.000000000000000000 ) ) ;
#23960 = ORIENTED_EDGE ( 'NONE', *, *, #10296, .F. ) ;
#23961 = DIRECTION ( 'NONE',  ( 1.000000000000000000, 0.000000000000000000, 0.000000000000000000 ) ) ;
#23962 = CARTESIAN_POINT ( 'NONE',  ( 118.6910030610041815, 140.0000000000000000, 100.0000000000000000 ) ) ;
#23963 = LINE ( 'NONE', #23678, #2500 ) ;
#23964 = CARTESIAN_POINT ( 'NONE',  ( 107.2624567859743792, 208.5673104118459378, -149.5176478624189542 ) ) ;
#23965 = VERTEX_POINT ( 'NONE', #3022 ) ;
#23966 = VECTOR ( 'NONE', #12518, 1000.000000000000114 ) ;
#23967 = CARTESIAN_POINT ( 'NONE',  ( 89.82706236707214487, 239.6935390654258242, -16.61376038145277434 ) ) ;
#23968 = ORIENTED_EDGE ( 'NONE', *, *, #7094, .T. ) ;
#23969 = CARTESIAN_POINT ( 'NONE',  ( -11.65927247860673255, 131.4491652140310407, -14.75293135532740152 ) ) ;
#23970 = ORIENTED_EDGE ( 'NONE', *, *, #11236, .T. ) ;
#23971 = VECTOR ( 'NONE', #26293, 1000.000000000000000 ) ;
#23972 = ORIENTED_EDGE ( 'NONE', *, *, #2589, .F. ) ;
#23973 = VECTOR ( 'NONE', #4553, 1000.000000000000114 ) ;
#23974 = ORIENTED_EDGE ( 'NONE', *, *, #23141, .F. ) ;
#23975 = ORIENTED_EDGE ( 'NONE', *, *, #27631, .T. ) ;
#23976 = CARTESIAN_POINT ( 'NONE',  ( -140.1213116003368668, 122.5384136796733827, -13.00000000000000000 ) ) ;
#23977 = DIRECTION ( 'NONE',  ( -0.000000000000000000, 0.000000000000000000, 1.000000000000000000 ) ) ;
#23978 = CARTESIAN_POINT ( 'NONE',  ( 157.9999999999996305, 283.6968751876750616, 45.00000000000000000 ) ) ;
#23979 = VECTOR ( 'NONE', #4569, 1000.000000000000000 ) ;
#23980 = CARTESIAN_POINT ( 'NONE',  ( 158.0000000000000853, 200.9369999399436892, 45.00000000000000000 ) ) ;
#23981 = CIRCLE ( 'NONE', #27192, 10.53396790234563518 ) ;
#23982 = EDGE_CURVE ( 'NONE', #5063, #606, #22992, .T. ) ;
#23983 = CARTESIAN_POINT ( 'NONE',  ( 158.0000000000010232, 108.1456246621830957, 45.00000000000000000 ) ) ;
#23984 = DIRECTION ( 'NONE',  ( 0.3897722486529259234, -0.9209112846414911902, 0.000000000000000000 ) ) ;
#23985 = VECTOR ( 'NONE', #10713, 1000.000000000000000 ) ;
#23986 = DIRECTION ( 'NONE',  ( 1.000000000000000000, 0.000000000000000000, -0.000000000000000000 ) ) ;
#23987 = CARTESIAN_POINT ( 'NONE',  ( 48.45469728424486533, 192.9461374953035033, -15.00000000000000000 ) ) ;
#23988 = ADVANCED_FACE ( 'NONE', ( #7493 ), #16258, .F. ) ;
#23989 = AXIS2_PLACEMENT_3D ( 'NONE', #16053, #18892, #25219 ) ;
#23990 = DIRECTION ( 'NONE',  ( -0.000000000000000000, -0.000000000000000000, -1.000000000000000000 ) ) ;
#23991 = FACE_OUTER_BOUND ( 'NONE', #9410, .T. ) ;
#23992 = LINE ( 'NONE', #19389, #2691 ) ;
#23993 = DIRECTION ( 'NONE',  ( 0.000000000000000000, 0.000000000000000000, -1.000000000000000000 ) ) ;
#23994 = DIRECTION ( 'NONE',  ( -0.000000000000000000, -0.000000000000000000, -1.000000000000000000 ) ) ;
#23995 = CARTESIAN_POINT ( 'NONE',  ( 157.4999999999998295, 218.7460624962465090, 45.00000000000000000 ) ) ;
#23997 = EDGE_LOOP ( 'NONE', ( #158, #11514, #25571, #27906, #19295, #10687 ) ) ;
#23996 = ORIENTED_EDGE ( 'NONE', *, *, #21129, .T. ) ;
#23998 = CARTESIAN_POINT ( 'NONE',  ( -173.6123854203675592, 113.7649492691934086, 27.03905483108168895 ) ) ;
#23999 = CARTESIAN_POINT ( 'NONE',  ( -17.24491960465745777, -18.01420295945611727, 95.00000000000000000 ) ) ;
#24000 = ORIENTED_EDGE ( 'NONE', *, *, #17717, .F. ) ;
#24001 = PRODUCT_CONTEXT ( 'NONE', #8003, 'mechanical' ) ;
#24002 = EDGE_LOOP ( 'NONE', ( #25418, #4013, #7823, #7001 ) ) ;
#24003 = AXIS2_PLACEMENT_3D ( 'NONE', #19870, #13417, #342 ) ;
#24004 = EDGE_LOOP ( 'NONE', ( #1861, #6719, #11734, #18701 ) ) ;
#24005 = AXIS2_PLACEMENT_3D ( 'NONE', #18589, #7677, #24781 ) ;
#24006 = CYLINDRICAL_SURFACE ( 'NONE', #17072, 30.00000000000000000 ) ;
#24007 = EDGE_CURVE ( 'NONE', #3920, #19657, #22852, .T. ) ;
#24008 = CARTESIAN_POINT ( 'NONE',  ( 158.0000000000008527, 123.7007497147323960, 45.00000000000000000 ) ) ;
#24009 = VERTEX_POINT ( 'NONE', #3296 ) ;
#24010 = VECTOR ( 'NONE', #7285, 1000.000000000000000 ) ;
#24011 = CARTESIAN_POINT ( 'NONE',  ( 113.4920585194047078, 104.4775165427241461, -100.0000000000000142 ) ) ;
#24012 = LINE ( 'NONE', #16834, #22888 ) ;
#24013 = ORIENTED_EDGE ( 'NONE', *, *, #3883, .F. ) ;
#24014 = EDGE_CURVE ( 'NONE', #7637, #28220, #20834, .T. ) ;
#24015 = CARTESIAN_POINT ( 'NONE',  ( -223.2197326358865723, 88.62327920559705774, 14.89134622796188445 ) ) ;
#24016 = ORIENTED_EDGE ( 'NONE', *, *, #20197, .F. ) ;
#24017 = DIRECTION ( 'NONE',  ( 0.000000000000000000, 0.000000000000000000, 1.000000000000000000 ) ) ;
#24018 = EDGE_CURVE ( 'NONE', #15118, #12495, #14928, .T. ) ;
#24019 = EDGE_CURVE ( 'NONE', #14062, #15041, #25703, .T. ) ;
#24020 = EDGE_CURVE ( 'NONE', #21204, #11039, #17086, .T. ) ;
#24021 = DIRECTION ( 'NONE',  ( 1.000000000000000000, 0.000000000000000000, -0.000000000000000000 ) ) ;
#24022 = CARTESIAN_POINT ( 'NONE',  ( 159.8564679241521276, 203.2015132085163600, -150.6165463336312769 ) ) ;
#24023 = VECTOR ( 'NONE', #1426, 1000.000000000000227 ) ;
#24024 = CARTESIAN_POINT ( 'NONE',  ( 2.399999999999999911, 0.000000000000000000, 0.000000000000000000 ) ) ;
#24025 = ORIENTED_EDGE ( 'NONE', *, *, #6020, .T. ) ;
#24026 = VECTOR ( 'NONE', #13695, 1000.000000000000000 ) ;
#24027 = CARTESIAN_POINT ( 'NONE',  ( 157.4999999999998579, 95.86018712840139244, 45.00000000000000000 ) ) ;
#24028 = CARTESIAN_POINT ( 'NONE',  ( 157.4999999999998579, 93.35231212089433939, -45.00000000000000000 ) ) ;
#24029 = CARTESIAN_POINT ( 'NONE',  ( 158.0000000000016485, 48.46449948952110987, -45.00000000000000000 ) ) ;
#24030 = TOROIDAL_SURFACE ( 'NONE', #7530, 7.509856658345970715, 10.53396790234564762 ) ;
#24031 = LINE ( 'NONE', #19992, #25417 ) ;
#24032 = ORIENTED_EDGE ( 'NONE', *, *, #13486, .F. ) ;
#24033 = CARTESIAN_POINT ( 'NONE',  ( -211.7373893208448692, -220.0000000000001421, -107.1635277725268196 ) ) ;
#24034 = DIRECTION ( 'NONE',  ( -1.000000000000000000, -2.312964634635742957E-16, 0.000000000000000000 ) ) ;
#24035 = FACE_OUTER_BOUND ( 'NONE', #11237, .T. ) ;
#24036 = VERTEX_POINT ( 'NONE', #5741 ) ;
#24037 =( NAMED_UNIT ( * ) PLANE_ANGLE_UNIT ( ) SI_UNIT ( $, .RADIAN. ) );
#24038 = SHAPE_REPRESENTATION ( 'Structural Component', ( #10637 ), #3285 ) ;
#24039 = ORIENTED_EDGE ( 'NONE', *, *, #26622, .F. ) ;
#24040 = FACE_OUTER_BOUND ( 'NONE', #21481, .T. ) ;
#24041 = CARTESIAN_POINT ( 'NONE',  ( -160.5161435040798494, 120.3804527765386467, -22.28951900308574707 ) ) ;
#24042 = ORIENTED_EDGE ( 'NONE', *, *, #743, .T. ) ;
#24043 = AXIS2_PLACEMENT_3D ( 'NONE', #24055, #4358, #6662 ) ;
#24044 = ORIENTED_EDGE ( 'NONE', *, *, #11513, .F. ) ;
#24045 = CARTESIAN_POINT ( 'NONE',  ( -113.6546414130708058, 71.26467278202298417, 82.82413405842315512 ) ) ;
#24046 = EDGE_CURVE ( 'NONE', #19744, #13525, #8025, .T. ) ;
#24047 = EDGE_CURVE ( 'NONE', #14163, #8537, #23558, .T. ) ;
#24048 = CARTESIAN_POINT ( 'NONE',  ( -71.37541315349507443, 230.0000000000000000, 15.00000000000000000 ) ) ;
#24049 = ORIENTED_EDGE ( 'NONE', *, *, #5150, .T. ) ;
#24050 = VERTEX_POINT ( 'NONE', #14946 ) ;
#24051 = VECTOR ( 'NONE', #20696, 1000.000000000000000 ) ;
#24052 = CARTESIAN_POINT ( 'NONE',  ( -33.96955706545894316, 128.1973378200279399, 17.41747935847348572 ) ) ;
#24053 = EDGE_CURVE ( 'NONE', #10285, #25999, #28132, .T. ) ;
#24054 = CARTESIAN_POINT ( 'NONE',  ( -175.0000000000000000, -170.0000000000001990, -69.99999999999998579 ) ) ;
#24055 = CARTESIAN_POINT ( 'NONE',  ( 134.9999999999998579, 220.0000000000000284, -122.9999999999999574 ) ) ;
#24056 = DIRECTION ( 'NONE',  ( -0.000000000000000000, -0.000000000000000000, -1.000000000000000000 ) ) ;
#24057 = LINE ( 'NONE', #13421, #23791 ) ;
#24058 = CARTESIAN_POINT ( 'NONE',  ( -209.9968668340340514, 60.57717296128767970, -21.99721431589914644 ) ) ;
#24059 = CARTESIAN_POINT ( 'NONE',  ( 158.0000000000000284, 205.9527499549551806, 45.00000000000000000 ) ) ;
#24060 = EDGE_CURVE ( 'NONE', #22186, #6357, #1292, .T. ) ;
#24061 = ORIENTED_EDGE ( 'NONE', *, *, #17505, .T. ) ;
#24062 = DIRECTION ( 'NONE',  ( 1.000000000000000000, 2.602085213965211135E-16, 0.000000000000000000 ) ) ;
#24063 = CARTESIAN_POINT ( 'NONE',  ( 157.4999999999994600, 216.2381874887387880, 45.00000000000000000 ) ) ;
#24064 = DIRECTION ( 'NONE',  ( -0.000000000000000000, -0.000000000000000000, -1.000000000000000000 ) ) ;
#24065 = CARTESIAN_POINT ( 'NONE',  ( 158.0000000000009379, 116.1771246922112653, -45.00000000000000000 ) ) ;
#24066 = ORIENTED_EDGE ( 'NONE', *, *, #6909, .T. ) ;
#24067 = AXIS2_PLACEMENT_3D ( 'NONE', #19873, #488, #13281 ) ;
#24068 = DIRECTION ( 'NONE',  ( 0.000000000000000000, -1.000000000000000000, 0.000000000000000000 ) ) ;
#24069 = DIRECTION ( 'NONE',  ( -1.000000000000000000, 1.850371707708594366E-15, 0.000000000000000000 ) ) ;
#24070 = CARTESIAN_POINT ( 'NONE',  ( -244.5479615644635771, 75.99513337129096158, -5.000000000000004441 ) ) ;
#24071 = LINE ( 'NONE', #23500, #2979 ) ;
#24072 = CARTESIAN_POINT ( 'NONE',  ( 122.6339745962156229, 200.5814157129576074, 45.00000000000000000 ) ) ;
#24073 = CARTESIAN_POINT ( 'NONE',  ( 125.3433571860710600, 197.9412384757604570, 84.99999999999995737 ) ) ;
#24074 = AXIS2_PLACEMENT_3D ( 'NONE', #12913, #8309, #1971 ) ;
#24075 = ORIENTED_EDGE ( 'NONE', *, *, #21790, .T. ) ;
#24076 = CARTESIAN_POINT ( 'NONE',  ( -207.5044420441008128, 75.59897387903035337, 43.94429683754297855 ) ) ;
#24077 = ORIENTED_EDGE ( 'NONE', *, *, #3145, .T. ) ;
#24078 = CARTESIAN_POINT ( 'NONE',  ( -263.2465583119826533, -166.4129100889759059, 109.9213744122507990 ) ) ;
#24079 = VERTEX_POINT ( 'NONE', #10341 ) ;
#24080 = ORIENTED_EDGE ( 'NONE', *, *, #13485, .F. ) ;
#24081 = DIRECTION ( 'NONE',  ( 0.8916010070294395629, -0.4528218681381114274, 0.000000000000000000 ) ) ;
#24082 = EDGE_CURVE ( 'NONE', #12779, #25488, #1595, .T. ) ;
#24083 = VECTOR ( 'NONE', #6975, 1000.000000000000000 ) ;
#24084 = VERTEX_POINT ( 'NONE', #8472 ) ;
#24085 = ORIENTED_EDGE ( 'NONE', *, *, #14232, .F. ) ;
#24086 = DIRECTION ( 'NONE',  ( 0.000000000000000000, -1.000000000000000000, 0.000000000000000000 ) ) ;
#24087 = VECTOR ( 'NONE', #5881, 1000.000000000000000 ) ;
#24088 = CARTESIAN_POINT ( 'NONE',  ( -101.3605996677730872, 134.2152826476940959, -15.56279420024448612 ) ) ;
#24089 = CARTESIAN_POINT ( 'NONE',  ( 103.8044331943677321, 239.2408796538006186, 26.67200500018185494 ) ) ;
#24090 = CARTESIAN_POINT ( 'NONE',  ( -37.82257053376181233, 36.92584315232891612, 99.00000000000000000 ) ) ;
#24091 = LINE ( 'NONE', #28235, #4552 ) ;
#24092 = AXIS2_PLACEMENT_3D ( 'NONE', #15891, #24636, #22047 ) ;
#24093 = CARTESIAN_POINT ( 'NONE',  ( -68.57415822541635464, 24.64876300893806160, 100.0000000000000000 ) ) ;
#24094 = FACE_OUTER_BOUND ( 'NONE', #12565, .T. ) ;
#24095 = CARTESIAN_POINT ( 'NONE',  ( 122.6339745962154808, 239.4185842870417389, 45.00000000000000000 ) ) ;
#24096 = EDGE_CURVE ( 'NONE', #25971, #7114, #19101, .T. ) ;
#24097 = EDGE_CURVE ( 'NONE', #28358, #17098, #11718, .T. ) ;
#24098 = DIRECTION ( 'NONE',  ( 1.000000000000000000, 0.000000000000000000, 0.000000000000000000 ) ) ;
#24099 = PLANE ( 'NONE',  #15856 ) ;
#24100 = EDGE_CURVE ( 'NONE', #3224, #24757, #10725, .T. ) ;
#24101 = DIRECTION ( 'NONE',  ( -0.000000000000000000, -0.000000000000000000, 1.000000000000000000 ) ) ;
#24102 = CARTESIAN_POINT ( 'NONE',  ( -200.0000000000000284, -91.18033988749901653, 0.000000000000000000 ) ) ;
#24103 = DIRECTION ( 'NONE',  ( 0.000000000000000000, 0.000000000000000000, -1.000000000000000000 ) ) ;
#24104 = ORIENTED_EDGE ( 'NONE', *, *, #21709, .T. ) ;
#24105 = CARTESIAN_POINT ( 'NONE',  ( -210.0000000000000284, -40.00000000000005684, -70.00000000000001421 ) ) ;
#24106 = CARTESIAN_POINT ( 'NONE',  ( -160.0000000000000284, 59.99999999999994316, -70.00000000000001421 ) ) ;
#24107 = PLANE ( 'NONE',  #16732 ) ;
#24108 = VECTOR ( 'NONE', #9248, 1000.000000000000000 ) ;
#24109 = DIRECTION ( 'NONE',  ( -0.000000000000000000, -0.000000000000000000, -1.000000000000000000 ) ) ;
#24110 = ORIENTED_EDGE ( 'NONE', *, *, #22618, .F. ) ;
#24111 = AXIS2_PLACEMENT_3D ( 'NONE', #11609, #24946, #14046 ) ;
#24112 = EDGE_CURVE ( 'NONE', #15680, #5949, #10626, .T. ) ;
#24113 = EDGE_CURVE ( 'NONE', #8240, #22485, #21397, .T. ) ;
#24114 = CARTESIAN_POINT ( 'NONE',  ( 192.5108452903457419, 172.8810361401565672, -45.00000000000000000 ) ) ;
#24115 = EDGE_LOOP ( 'NONE', ( #8338, #25549, #8710, #6355 ) ) ;
#24116 = VERTEX_POINT ( 'NONE', #3867 ) ;
#24117 = VECTOR ( 'NONE', #38, 1000.000000000000000 ) ;
#24118 = VERTEX_POINT ( 'NONE', #27705 ) ;
#24119 = ORIENTED_EDGE ( 'NONE', *, *, #27346, .F. ) ;
#24120 = VERTEX_POINT ( 'NONE', #12510 ) ;
#24121 = ORIENTED_EDGE ( 'NONE', *, *, #14051, .T. ) ;
#24122 = CARTESIAN_POINT ( 'NONE',  ( 157.4999999999998579, 178.6200623761337738, 45.00000000000000000 ) ) ;
#24123 = DIRECTION ( 'NONE',  ( 0.2066290158914688702, 0.9784193629480781862, 0.000000000000000000 ) ) ;
#24124 = CIRCLE ( 'NONE', #18159, 5.999999999999991118 ) ;
#24125 = AXIS2_PLACEMENT_3D ( 'NONE', #5055, #2908, #11691 ) ;
#24126 = DIRECTION ( 'NONE',  ( 1.000000000000000000, 0.000000000000000000, -0.000000000000000000 ) ) ;
#24127 = EDGE_CURVE ( 'NONE', #14873, #2828, #19244, .T. ) ;
#24128 = CARTESIAN_POINT ( 'NONE',  ( -223.9727688501994578, 61.67225750692129793, 20.13450274023654529 ) ) ;
#24129 = CARTESIAN_POINT ( 'NONE',  ( 232.4999999999996305, 133.0668745871126930, -36.86484227207694886 ) ) ;
#24130 = DIRECTION ( 'NONE',  ( 0.000000000000000000, 0.000000000000000000, -1.000000000000000000 ) ) ;
#24131 = ADVANCED_FACE ( 'NONE', ( #1575 ), #8183, .F. ) ;
#24132 = CARTESIAN_POINT ( 'NONE',  ( 187.4999999999996305, 494.4107529906318632, 74.99999999999997158 ) ) ;
#24133 = VECTOR ( 'NONE', #23954, 1000.000000000000000 ) ;
#24134 = DIRECTION ( 'NONE',  ( 1.000000000000000000, 0.000000000000000000, 0.000000000000000000 ) ) ;
#24135 = CARTESIAN_POINT ( 'NONE',  ( 119.9999999999998863, 330.0000000000000000, -100.0000000000000142 ) ) ;
#24136 = LINE ( 'NONE', #26413, #4507 ) ;
#24137 = DIRECTION ( 'NONE',  ( 1.000000000000000000, 0.000000000000000000, 0.000000000000000000 ) ) ;
#24138 = CARTESIAN_POINT ( 'NONE',  ( -180.5664960625764195, 109.3611654016444419, 31.00115732394728241 ) ) ;
#24139 = CARTESIAN_POINT ( 'NONE',  ( 187.4999999999996305, 40.68693696324645970, 45.00000000000000000 ) ) ;
#24141 = ORIENTED_EDGE ( 'NONE', *, *, #16297, .F. ) ;
#24140 = VERTEX_POINT ( 'NONE', #8329 ) ;
#24142 = EDGE_CURVE ( 'NONE', #12217, #1063, #23844, .T. ) ;
#24143 = CARTESIAN_POINT ( 'NONE',  ( -164.2459188995896682, 118.6424907086743161, 23.77112046045245108 ) ) ;
#24144 = CARTESIAN_POINT ( 'NONE',  ( -203.7123084376263762, 92.59051442877377269, -28.49533127386492026 ) ) ;
#24145 = VERTEX_POINT ( 'NONE', #24132 ) ;
#24146 = ORIENTED_EDGE ( 'NONE', *, *, #7995, .F. ) ;
#24148 = EDGE_CURVE ( 'NONE', #19656, #24242, #10913, .T. ) ;
#24147 = VECTOR ( 'NONE', #2583, 999.9999999999998863 ) ;
#24150 = EDGE_CURVE ( 'NONE', #12678, #23433, #7025, .T. ) ;
#24149 = ORIENTED_EDGE ( 'NONE', *, *, #5389, .F. ) ;
#24151 = FACE_OUTER_BOUND ( 'NONE', #18333, .T. ) ;
#24152 = LINE ( 'NONE', #10505, #12691 ) ;
#24153 = ORIENTED_EDGE ( 'NONE', *, *, #16500, .F. ) ;
#24154 = EDGE_CURVE ( 'NONE', #26356, #15878, #6454, .T. ) ;
#24155 = CIRCLE ( 'NONE', #23697, 5.999999999999977796 ) ;
#24156 = CARTESIAN_POINT ( 'NONE',  ( 116.3389527600916722, 113.0483370489294686, -100.0000000000000142 ) ) ;
#24157 = DIRECTION ( 'NONE',  ( 1.000000000000000000, 0.000000000000000000, 0.000000000000000000 ) ) ;
#24158 = ORIENTED_EDGE ( 'NONE', *, *, #27140, .F. ) ;
#24159 = CARTESIAN_POINT ( 'NONE',  ( -215.4422302146570871, 87.87472848447453089, 19.21920766392561575 ) ) ;
#24160 = CYLINDRICAL_SURFACE ( 'NONE', #20799, 5.999999999999991118 ) ;
#24161 = CARTESIAN_POINT ( 'NONE',  ( 157.9999999999996589, 276.6811251726610976, 45.00000000000000000 ) ) ;
#24162 = EDGE_CURVE ( 'NONE', #21449, #8519, #5278, .T. ) ;
#24163 = CARTESIAN_POINT ( 'NONE',  ( 157.7131785260345112, 200.4010886758948686, -147.1195141158909223 ) ) ;
#24164 = VECTOR ( 'NONE', #11108, 1000.000000000000227 ) ;
#24165 = ORIENTED_EDGE ( 'NONE', *, *, #11211, .T. ) ;
#24166 = FACE_OUTER_BOUND ( 'NONE', #933, .T. ) ;
#24167 = LINE ( 'NONE', #21865, #23429 ) ;
#24168 = B_SPLINE_CURVE_WITH_KNOTS ( 'NONE', 3,
 ( #3069, #10256, #6354, #19577, #3775, #23462, #15135, #25747, #3916, #19013, #23891, #28316, #4196, #23744, #8236, #12564, #21442, #8661, #4339, #12842, #8378, #27758, #5934, #16995, #10534, #4053, #14708, #12987, #17417, #1756 ),
 .UNSPECIFIED., .F., .F.,
 ( 4, 2, 2, 2, 2, 2, 2, 2, 2, 2, 2, 2, 2, 2, 4 ),
 ( 0.000000000000000000, 0.004470907159210596622, 0.005588633949013227346, 0.006706360738815858938, 0.008941814318421193244, 0.01117726789802652755, 0.01341272147763186012, 0.01788362863684252527, 0.02011908221644785957, 0.02235453579605319388, 0.02682544295526392841, 0.02906089653486926619, 0.03129635011447460397, 0.03353180369407994521, 0.03576725727368528646 ),
 .UNSPECIFIED. ) ;
#24169 = CARTESIAN_POINT ( 'NONE',  ( 79.99999999999992895, 110.0000000000000000, -70.00000000000001421 ) ) ;
#24170 = CARTESIAN_POINT ( 'NONE',  ( 367.4999999999996021, 44.41075299063184900, 1.850330238640837654E-14 ) ) ;
#24171 = ORIENTED_EDGE ( 'NONE', *, *, #7742, .T. ) ;
#24172 = CARTESIAN_POINT ( 'NONE',  ( -25.39999999999996305, 0.000000000000000000, 5.000000000000000000 ) ) ;
#24173 = CARTESIAN_POINT ( 'NONE',  ( 158.0000000000003979, 168.8424998498591663, -45.00000000000000000 ) ) ;
#24174 = DIRECTION ( 'NONE',  ( -0.000000000000000000, 1.000000000000000000, -0.000000000000000000 ) ) ;
#24175 = VERTEX_POINT ( 'NONE', #284 ) ;
#24176 = ORIENTED_EDGE ( 'NONE', *, *, #10618, .F. ) ;
#24177 = EDGE_CURVE ( 'NONE', #5808, #12260, #2276, .T. ) ;
#24178 = CARTESIAN_POINT ( 'NONE',  ( 134.9999999999998579, 220.0000000000000284, 100.0000000000000142 ) ) ;
#24179 = EDGE_CURVE ( 'NONE', #4619, #1981, #15517, .T. ) ;
#24180 = CARTESIAN_POINT ( 'NONE',  ( -188.6978706431725357, 104.3090321516409631, -31.95341200857410158 ) ) ;
#24181 = ORIENTED_EDGE ( 'NONE', *, *, #12839, .F. ) ;
#24182 = CIRCLE ( 'NONE', #19129, 16.46313063346208239 ) ;
#24183 = EDGE_LOOP ( 'NONE', ( #6817, #21992, #23060, #16322, #24790 ) ) ;
#24184 = FACE_OUTER_BOUND ( 'NONE', #19601, .T. ) ;
#24185 = LINE ( 'NONE', #13275, #8889 ) ;
#24186 = VERTEX_POINT ( 'NONE', #15230 ) ;
#24187 = ORIENTED_EDGE ( 'NONE', *, *, #20516, .F. ) ;
#24188 = CARTESIAN_POINT ( 'NONE',  ( -305.0000000000001137, -152.0000000000000284, -59.99999999999987210 ) ) ;
#24189 = DIRECTION ( 'NONE',  ( 0.000000000000000000, -1.000000000000000000, 0.000000000000000000 ) ) ;
#24190 = DIRECTION ( 'NONE',  ( -0.000000000000000000, 1.000000000000000000, -1.387778780781445429E-16 ) ) ;
#24191 = DIRECTION ( 'NONE',  ( 0.000000000000000000, 0.000000000000000000, -1.000000000000000000 ) ) ;
#24192 = CARTESIAN_POINT ( 'NONE',  ( 158.0000000000014211, 71.03537455708449500, 45.00000000000000000 ) ) ;
#24193 = CARTESIAN_POINT ( 'NONE',  ( -261.1919288306253293, -171.9377729149742038, 105.0000000000000142 ) ) ;
#24194 = CARTESIAN_POINT ( 'NONE',  ( -210.0000000000000568, -220.0000000000000853, -90.87829376371895762 ) ) ;
#24195 = EDGE_LOOP ( 'NONE', ( #4382, #4605, #25299, #17713 ) ) ;
#24196 = CARTESIAN_POINT ( 'NONE',  ( 157.4999999999998579, 171.0964373536126573, 45.00000000000000000 ) ) ;
#24197 = FACE_OUTER_BOUND ( 'NONE', #15694, .T. ) ;
#24198 = LINE ( 'NONE', #24628, #8672 ) ;
#24199 = CARTESIAN_POINT ( 'NONE',  ( 267.4999999999996021, 194.4107529906318064, -75.35061095560291733 ) ) ;
#24200 = CIRCLE ( 'NONE', #11831, 30.00000000000000000 ) ;
#24201 = VERTEX_POINT ( 'NONE', #11199 ) ;
#24202 = DIRECTION ( 'NONE',  ( 0.8916010070298563406, 0.4528218681372909171, 0.000000000000000000 ) ) ;
#24203 = ORIENTED_EDGE ( 'NONE', *, *, #10194, .T. ) ;
#24204 = FACE_OUTER_BOUND ( 'NONE', #15581, .T. ) ;
#24205 = CARTESIAN_POINT ( 'NONE',  ( 157.4999999999998579, 191.1594374136689964, 45.00000000000000000 ) ) ;
#24206 = CARTESIAN_POINT ( 'NONE',  ( -40.40953891503691153, 0.000000000000000000, 99.00000000000000000 ) ) ;
#24207 = ORIENTED_EDGE ( 'NONE', *, *, #1373, .F. ) ;
#24208 = LINE ( 'NONE', #24638, #21171 ) ;
#24209 = SURFACE_STYLE_USAGE ( .BOTH. , #26352 ) ;
#24210 = ORIENTED_EDGE ( 'NONE', *, *, #20957, .T. ) ;
#24211 = EDGE_CURVE ( 'NONE', #11551, #15954, #19952, .T. ) ;
#24212 = CARTESIAN_POINT ( 'NONE',  ( 157.4999999999994600, 213.7303124812313513, 45.00000000000000000 ) ) ;
#24213 = ORIENTED_EDGE ( 'NONE', *, *, #27341, .T. ) ;
#24214 = EDGE_CURVE ( 'NONE', #4314, #5835, #8616, .T. ) ;
#24215 = CARTESIAN_POINT ( 'NONE',  ( -262.5800650587033260, -171.5970377885955145, 95.00000000000000000 ) ) ;
#24216 = ORIENTED_EDGE ( 'NONE', *, *, #21988, .F. ) ;
#24217 = ORIENTED_EDGE ( 'NONE', *, *, #20062, .F. ) ;
#24218 = CARTESIAN_POINT ( 'NONE',  ( 157.4999999999998010, 236.3011875487955251, 45.00000000000000000 ) ) ;
#24219 = AXIS2_PLACEMENT_3D ( 'NONE', #14079, #568, #22691 ) ;
#24220 = ORIENTED_EDGE ( 'NONE', *, *, #26001, .T. ) ;
#24221 = ORIENTED_EDGE ( 'NONE', *, *, #27794, .T. ) ;
#24222 = CARTESIAN_POINT ( 'NONE',  ( -310.0000000000001137, -157.0000000000000284, -59.99999999999987210 ) ) ;
#24223 = CARTESIAN_POINT ( 'NONE',  ( 91.17299970895479078, 230.3777436784795043, 17.14176051628196262 ) ) ;
#24224 = CARTESIAN_POINT ( 'NONE',  ( 167.4999999999996589, -5.589247009368136787, -84.99999999999995737 ) ) ;
#24225 = CARTESIAN_POINT ( 'NONE',  ( 157.4999999999998579, 123.4468122109788482, -45.00000000000000000 ) ) ;
#24226 = PLANE ( 'NONE',  #7805 ) ;
#24227 = LINE ( 'NONE', #4261, #24554 ) ;
#24228 = DIRECTION ( 'NONE',  ( -0.000000000000000000, -0.000000000000000000, -1.000000000000000000 ) ) ;
#24229 = AXIS2_PLACEMENT_3D ( 'NONE', #24677, #7439, #1105 ) ;
#24230 = CARTESIAN_POINT ( 'NONE',  ( -160.0000000000000284, 59.99999999999994316, -45.00000000000000000 ) ) ;
#24231 = DIRECTION ( 'NONE',  ( 0.8916010070293783896, -0.4528218681382319422, 0.000000000000000000 ) ) ;
#24232 = FACE_BOUND ( 'NONE', #22810, .T. ) ;
#24233 = CARTESIAN_POINT ( 'NONE',  ( 217.4999999999996305, -5.589247009368160768, 100.0000000000000142 ) ) ;
#24234 = VERTEX_POINT ( 'NONE', #28273 ) ;
#24235 = DIRECTION ( 'NONE',  ( -1.000000000000000000, -0.000000000000000000, 0.000000000000000000 ) ) ;
#24236 = TOROIDAL_SURFACE ( 'NONE', #20111, 30.49120955644046660, 2.000000000000000000 ) ;
#24237 = EDGE_CURVE ( 'NONE', #13747, #1725, #23628, .T. ) ;
#24238 = AXIS2_PLACEMENT_3D ( 'NONE', #21152, #1473, #9961 ) ;
#24239 = DIRECTION ( 'NONE',  ( -0.000000000000000000, -0.000000000000000000, -1.000000000000000000 ) ) ;
#24240 = CARTESIAN_POINT ( 'NONE',  ( -63.57415822541634043, 0.000000000000000000, 100.0000000000000000 ) ) ;
#24241 = CARTESIAN_POINT ( 'NONE',  ( 106.8486790052090782, 209.6310448320832904, -141.8266621613457517 ) ) ;
#24242 = VERTEX_POINT ( 'NONE', #424 ) ;
#24243 = CARTESIAN_POINT ( 'NONE',  ( 107.7175597583449189, 250.4128021204703600, -33.27520275791160742 ) ) ;
#24244 = ORIENTED_EDGE ( 'NONE', *, *, #17079, .F. ) ;
#24245 = ADVANCED_FACE ( 'NONE', ( #26129 ), #15809, .F. ) ;
#24246 = VERTEX_POINT ( 'NONE', #23987 ) ;
#24247 = ADVANCED_BREP_SHAPE_REPRESENTATION ( '', ( #18502, #10637 ), #25313 ) ;
#24248 = ORIENTED_EDGE ( 'NONE', *, *, #22198, .F. ) ;
#24249 = EDGE_CURVE ( 'NONE', #23784, #1799, #4147, .T. ) ;
#24250 = AXIS2_PLACEMENT_3D ( 'NONE', #22856, #3162, #19987 ) ;
#24251 = ORIENTED_EDGE ( 'NONE', *, *, #24100, .F. ) ;
#24252 = ORIENTED_EDGE ( 'NONE', *, *, #3351, .T. ) ;
#24253 = ORIENTED_EDGE ( 'NONE', *, *, #14639, .T. ) ;
#24254 = DIRECTION ( 'NONE',  ( 0.000000000000000000, -1.000000000000000000, 0.000000000000000000 ) ) ;
#24255 = AXIS2_PLACEMENT_3D ( 'NONE', #21898, #2205, #19740 ) ;
#24256 = AXIS2_PLACEMENT_3D ( 'NONE', #22753, #11843, #9680 ) ;
#24257 = FACE_OUTER_BOUND ( 'NONE', #18503, .T. ) ;
#24258 = DIRECTION ( 'NONE',  ( -0.000000000000000000, -0.000000000000000000, -1.000000000000000000 ) ) ;
#24259 = EDGE_CURVE ( 'NONE', #24930, #15707, #1997, .T. ) ;
#24260 = CARTESIAN_POINT ( 'NONE',  ( -198.1081924558745584, 61.84288891412396083, 30.88603804298443833 ) ) ;
#24261 = DIRECTION ( 'NONE',  ( -0.000000000000000000, -0.000000000000000000, -1.000000000000000000 ) ) ;
#24262 = DIRECTION ( 'NONE',  ( -0.2588190451025121908, 0.9659258262890705327, 0.000000000000000000 ) ) ;
#24263 = CARTESIAN_POINT ( 'NONE',  ( 157.4999999999998579, 120.9389372034718093, 45.00000000000000000 ) ) ;
#24264 = CARTESIAN_POINT ( 'NONE',  ( 158.0000000000016485, 48.46449948952110987, 45.00000000000000000 ) ) ;
#24265 = PLANE ( 'NONE',  #27861 ) ;
#24266 = CARTESIAN_POINT ( 'NONE',  ( -175.0000000000000000, -120.0000000000001847, -69.99999999999998579 ) ) ;
#24267 = ADVANCED_FACE ( 'NONE', ( #4717 ), #4299, .T. ) ;
#24269 = CARTESIAN_POINT ( 'NONE',  ( -3.472619751711179426, 132.8132803667743644, 15.86983229809730389 ) ) ;
#24268 = VECTOR ( 'NONE', #35, 1000.000000000000000 ) ;
#24270 = DIRECTION ( 'NONE',  ( -0.8916010070296935819, 0.4528218681376112165, 0.000000000000000000 ) ) ;
#24271 = DIRECTION ( 'NONE',  ( -1.000000000000000000, -1.321694076934710155E-16, 0.000000000000000000 ) ) ;
#24272 = FACE_OUTER_BOUND ( 'NONE', #15220, .T. ) ;
#24274 = ORIENTED_EDGE ( 'NONE', *, *, #20149, .F. ) ;
#24273 = VERTEX_POINT ( 'NONE', #2137 ) ;
#24275 = CARTESIAN_POINT ( 'NONE',  ( -230.2711638029755932, 89.63949233591094412, -15.23082775398237487 ) ) ;
#24276 = CIRCLE ( 'NONE', #19231, 1.999999999999996891 ) ;
#24277 = CARTESIAN_POINT ( 'NONE',  ( -206.1524755872160881, 90.88176262967643027, -27.63232739364782020 ) ) ;
#24278 = ORIENTED_EDGE ( 'NONE', *, *, #12998, .T. ) ;
#24279 = VERTEX_POINT ( 'NONE', #6531 ) ;
#24280 = ORIENTED_EDGE ( 'NONE', *, *, #19163, .T. ) ;
#24281 = EDGE_CURVE ( 'NONE', #21312, #26943, #20093, .T. ) ;
#24282 = LINE ( 'NONE', #17964, #3297 ) ;
#24283 = ADVANCED_FACE ( 'NONE', ( #4433 ), #17943, .F. ) ;
#24284 = CARTESIAN_POINT ( 'NONE',  ( -160.8326600028555617, 120.2355194873574931, 21.37420696376539908 ) ) ;
#24285 = ORIENTED_EDGE ( 'NONE', *, *, #14133, .F. ) ;
#24286 = DIRECTION ( 'NONE',  ( -3.469446951953614189E-16, 1.000000000000000000, -0.000000000000000000 ) ) ;
#24287 = VECTOR ( 'NONE', #24878, 1000.000000000000227 ) ;
#24288 = DIRECTION ( 'NONE',  ( 0.7440215159219069063, 0.6681556583950086781, 0.000000000000000000 ) ) ;
#24289 = AXIS2_PLACEMENT_3D ( 'NONE', #23439, #18988, #25729 ) ;
#24290 = EDGE_LOOP ( 'NONE', ( #3395, #23972, #2834, #19281 ) ) ;
#24291 = CARTESIAN_POINT ( 'NONE',  ( -209.6188097997069519, 88.33184316452725682, 25.56917691525033121 ) ) ;
#24292 = CARTESIAN_POINT ( 'NONE',  ( -212.3316009019935962, -218.3936534609811133, 106.8607414965052556 ) ) ;
#24293 = EDGE_CURVE ( 'NONE', #4321, #18978, #26548, .T. ) ;
#24294 = CARTESIAN_POINT ( 'NONE',  ( 158.0000000000015064, 63.00387452705633251, 45.00000000000000000 ) ) ;
#24295 = CARTESIAN_POINT ( 'NONE',  ( 159.5493656458986322, 202.7558958333859209, -139.6178255645964441 ) ) ;
#24297 = EDGE_CURVE ( 'NONE', #5984, #2640, #25445, .T. ) ;
#24296 = CIRCLE ( 'NONE', #17887, 10.53396790234564762 ) ;
#24298 = ORIENTED_EDGE ( 'NONE', *, *, #5358, .F. ) ;
#24299 = PLANE ( 'NONE',  #13696 ) ;
#24300 = EDGE_CURVE ( 'NONE', #12920, #170, #3127, .T. ) ;
#24301 = CARTESIAN_POINT ( 'NONE',  ( -217.6530384384032573, 140.9974917369195566, -15.00000000000000000 ) ) ;
#24302 = PLANE ( 'NONE',  #14334 ) ;
#24303 = LINE ( 'NONE', #464, #21288 ) ;
#24304 = ORIENTED_EDGE ( 'NONE', *, *, #26114, .T. ) ;
#24305 = CARTESIAN_POINT ( 'NONE',  ( -212.1902760358752289, -220.0000000000001137, -105.8132860232897627 ) ) ;
#24306 = VECTOR ( 'NONE', #10276, 1000.000000000000000 ) ;
#24307 = CARTESIAN_POINT ( 'NONE',  ( -236.8667578982872044, 138.8517089611673043, 15.00000000000000000 ) ) ;
#24308 = CARTESIAN_POINT ( 'NONE',  ( 158.0000000000006537, 143.2558747672816821, 45.00000000000000000 ) ) ;
#24309 = ORIENTED_EDGE ( 'NONE', *, *, #22265, .F. ) ;
#24310 = VERTEX_POINT ( 'NONE', #27127 ) ;
#24311 = CIRCLE ( 'NONE', #3679, 10.71881775658151170 ) ;
#24312 = DIRECTION ( 'NONE',  ( -0.7730186417261840637, -0.6343833064826071011, 0.000000000000000000 ) ) ;
#24313 = CYLINDRICAL_SURFACE ( 'NONE', #12673, 30.00000000000000000 ) ;
#24314 = ORIENTED_EDGE ( 'NONE', *, *, #27982, .F. ) ;
#24315 = ORIENTED_EDGE ( 'NONE', *, *, #2306, .F. ) ;
#24316 = CARTESIAN_POINT ( 'NONE',  ( -111.6450422266150326, 69.94128127818710539, 82.90302649402674717 ) ) ;
#24317 = CARTESIAN_POINT ( 'NONE',  ( -71.37541315349507443, 150.2892445414773590, 5.000000000000002665 ) ) ;
#24318 = VERTEX_POINT ( 'NONE', #26848 ) ;
#24319 = ORIENTED_EDGE ( 'NONE', *, *, #15619, .T. ) ;
#24320 = DIRECTION ( 'NONE',  ( -0.8916010070296429557, -0.4528218681377111920, 0.000000000000000000 ) ) ;
#24321 = VECTOR ( 'NONE', #18303, 1000.000000000000000 ) ;
#24322 = DIRECTION ( 'NONE',  ( 0.000000000000000000, 0.000000000000000000, 1.000000000000000000 ) ) ;
#24323 = CARTESIAN_POINT ( 'NONE',  ( 158.0000000000004263, 166.3346248423521274, -45.00000000000000000 ) ) ;
#24324 = CARTESIAN_POINT ( 'NONE',  ( 158.0000000000014495, 68.01962454207041731, 45.00000000000000000 ) ) ;
#24325 = EDGE_CURVE ( 'NONE', #11442, #24784, #7737, .T. ) ;
#24326 = LINE ( 'NONE', #2481, #25155 ) ;
#24327 = ADVANCED_FACE ( 'NONE', ( #5152 ), #22689, .F. ) ;
#24328 = CARTESIAN_POINT ( 'NONE',  ( -208.6311953968240687, 71.65302225189010699, -39.58319495383710773 ) ) ;
#24329 = AXIS2_PLACEMENT_3D ( 'NONE', #23743, #17138, #12986 ) ;
#24330 = DIRECTION ( 'NONE',  ( -0.8379557447115656421, -0.5457381880580516320, 0.000000000000000000 ) ) ;
#24331 = ORIENTED_EDGE ( 'NONE', *, *, #5748, .T. ) ;
#24332 = DIRECTION ( 'NONE',  ( -0.8916010070295719014, -0.4528218681378510246, 0.000000000000000000 ) ) ;
#24333 = CARTESIAN_POINT ( 'NONE',  ( 157.4999999999998010, 236.3011875487955251, 45.00000000000000000 ) ) ;
#24334 = FACE_OUTER_BOUND ( 'NONE', #12350, .T. ) ;
#24335 = DIRECTION ( 'NONE',  ( 0.000000000000000000, 0.000000000000000000, 1.000000000000000000 ) ) ;
#24336 = ORIENTED_EDGE ( 'NONE', *, *, #3407, .T. ) ;
#24337 = FACE_OUTER_BOUND ( 'NONE', #11720, .T. ) ;
#24338 = EDGE_LOOP ( 'NONE', ( #21424, #8343, #478, #16656 ) ) ;
#24339 = CARTESIAN_POINT ( 'NONE',  ( 157.9999999999996589, 271.6653751576470768, -45.00000000000000000 ) ) ;
#24340 = DIRECTION ( 'NONE',  ( 0.8916010070293383105, -0.4528218681383106015, 0.000000000000000000 ) ) ;
#24341 = CARTESIAN_POINT ( 'NONE',  ( 136.3643978939877570, 249.9695740037962821, -150.8460904732142751 ) ) ;
#24342 = ORIENTED_EDGE ( 'NONE', *, *, #9290, .T. ) ;
#24343 = FACE_OUTER_BOUND ( 'NONE', #3007, .T. ) ;
#24344 = ORIENTED_EDGE ( 'NONE', *, *, #1654, .F. ) ;
#24345 = CIRCLE ( 'NONE', #26637, 22.49999999999999289 ) ;
#24346 = CARTESIAN_POINT ( 'NONE',  ( -210.0000000000000568, -220.0000000000000853, 90.00000000000002842 ) ) ;
#24347 = VERTEX_POINT ( 'NONE', #711 ) ;
#24348 = CARTESIAN_POINT ( 'NONE',  ( -275.9932544989950998, -170.0000000000001705, 91.21518331976510296 ) ) ;
#24349 = ORIENTED_EDGE ( 'NONE', *, *, #15652, .T. ) ;
#24350 = VERTEX_POINT ( 'NONE', #2850 ) ;
#24351 = PLANE ( 'NONE',  #7638 ) ;
#24352 = ORIENTED_EDGE ( 'NONE', *, *, #27948, .F. ) ;
#24353 = VECTOR ( 'NONE', #12833, 1000.000000000000000 ) ;
#24354 = ADVANCED_FACE ( 'NONE', ( #20806 ), #18094, .F. ) ;
#24355 = ORIENTED_EDGE ( 'NONE', *, *, #21052, .F. ) ;
#24356 = ORIENTED_EDGE ( 'NONE', *, *, #14332, .F. ) ;
#24357 = CARTESIAN_POINT ( 'NONE',  ( -218.8273392347107063, 140.3457761587386869, 14.99191580167233973 ) ) ;
#24358 = CARTESIAN_POINT ( 'NONE',  ( 91.79864198314062662, 239.6982472080604794, 17.32810371389381388 ) ) ;
#24359 = CARTESIAN_POINT ( 'NONE',  ( -210.0000000000000284, -40.00000000000005684, 100.0000000000000142 ) ) ;
#24360 = ADVANCED_FACE ( 'NONE', ( #1124 ), #13571, .T. ) ;
#24361 = DIRECTION ( 'NONE',  ( -1.000000000000000000, 0.000000000000000000, -0.000000000000000000 ) ) ;
#24362 = EDGE_CURVE ( 'NONE', #4407, #16727, #10065, .T. ) ;
#24363 = EDGE_CURVE ( 'NONE', #1132, #19895, #9757, .T. ) ;
#24364 = DIRECTION ( 'NONE',  ( -0.8916010070294503320, -0.4528218681380901667, 0.000000000000000000 ) ) ;
#24365 = CARTESIAN_POINT ( 'NONE',  ( -260.0000000000001137, -152.0000000000000284, 95.00000000000004263 ) ) ;
#24366 = DIRECTION ( 'NONE',  ( -0.000000000000000000, -0.000000000000000000, 1.000000000000000000 ) ) ;
#24367 = CIRCLE ( 'NONE', #26207, 24.07986109634097005 ) ;
#24368 = ADVANCED_FACE ( 'NONE', ( #7315 ), #24841, .F. ) ;
#24369 = CARTESIAN_POINT ( 'NONE',  ( 217.4999999999996305, 133.0668745871126930, 36.86484227207694886 ) ) ;
#24370 = CARTESIAN_POINT ( 'NONE',  ( -260.0000000000001137, -157.0000000000000284, 60.00000000000002132 ) ) ;
#24371 = CARTESIAN_POINT ( 'NONE',  ( 115.6411010564591777, 231.4666050640012429, -99.00000000000001421 ) ) ;
#24372 = DIRECTION ( 'NONE',  ( -0.000000000000000000, -0.000000000000000000, -1.000000000000000000 ) ) ;
#24373 = FACE_OUTER_BOUND ( 'NONE', #15920, .T. ) ;
#24374 = VERTEX_POINT ( 'NONE', #3551 ) ;
#24375 = DIRECTION ( 'NONE',  ( -0.000000000000000000, -0.000000000000000000, -1.000000000000000000 ) ) ;
#24376 = CIRCLE ( 'NONE', #977, 30.00000000000000000 ) ;
#24377 = LINE ( 'NONE', #686, #22927 ) ;
#24378 = DIRECTION ( 'NONE',  ( -0.000000000000000000, 0.000000000000000000, -1.000000000000000000 ) ) ;
#24379 = DIRECTION ( 'NONE',  ( 1.000000000000000000, 0.000000000000000000, 0.000000000000000000 ) ) ;
#24380 = ORIENTED_EDGE ( 'NONE', *, *, #25655, .T. ) ;
#24381 = CARTESIAN_POINT ( 'NONE',  ( 157.4999999999998579, 48.21056198576756202, 45.00000000000000000 ) ) ;
#24382 = VERTEX_POINT ( 'NONE', #25534 ) ;
#24383 =( LENGTH_UNIT ( ) NAMED_UNIT ( * ) SI_UNIT ( .MILLI., .METRE. ) );
#24384 = ORIENTED_EDGE ( 'NONE', *, *, #15315, .F. ) ;
#24385 = ORIENTED_EDGE ( 'NONE', *, *, #25655, .F. ) ;
#24386 = VECTOR ( 'NONE', #918, 1000.000000000000000 ) ;
#24387 = ORIENTED_EDGE ( 'NONE', *, *, #9752, .T. ) ;
#24388 = VERTEX_POINT ( 'NONE', #10453 ) ;
#24389 = ORIENTED_EDGE ( 'NONE', *, *, #6137, .T. ) ;
#24390 = CIRCLE ( 'NONE', #11106, 10.00000000000000888 ) ;
#24391 = EDGE_LOOP ( 'NONE', ( #14814, #15988, #19093 ) ) ;
#24392 = AXIS2_PLACEMENT_3D ( 'NONE', #9972, #1625, #5799 ) ;
#24393 = DIRECTION ( 'NONE',  ( 0.000000000000000000, -1.000000000000000000, 0.000000000000000000 ) ) ;
#24394 = CARTESIAN_POINT ( 'NONE',  ( 0.000000000000000000, 242.9999999999997158, 45.00000000000000000 ) ) ;
#24395 = EDGE_CURVE ( 'NONE', #23197, #17312, #25398, .T. ) ;
#24396 = AXIS2_PLACEMENT_3D ( 'NONE', #9903, #18798, #7879 ) ;
#24397 = EDGE_CURVE ( 'NONE', #26863, #19837, #20342, .T. ) ;
#24398 = EDGE_CURVE ( 'NONE', #23789, #9022, #19073, .T. ) ;
#24399 = DIRECTION ( 'NONE',  ( 0.9784193629480781862, -0.2066290158914688702, 0.000000000000000000 ) ) ;
#24400 = DIRECTION ( 'NONE',  ( 0.000000000000000000, -1.000000000000000000, 0.000000000000000000 ) ) ;
#24401 = CARTESIAN_POINT ( 'NONE',  ( -215.3329573320907571, 58.91837420258404023, 30.17944279517852024 ) ) ;
#24402 = CARTESIAN_POINT ( 'NONE',  ( 137.6105238444007455, 239.8288972274759203, 45.00000000000000000 ) ) ;
#24403 = DIRECTION ( 'NONE',  ( 0.9659258262890706437, 0.2588190451025122463, -0.000000000000000000 ) ) ;
#24404 = EDGE_CURVE ( 'NONE', #13313, #14722, #5716, .T. ) ;
#24405 = CARTESIAN_POINT ( 'NONE',  ( -221.3650667873343139, -91.18033988749901653, 14.94182580522077330 ) ) ;
#24406 = CARTESIAN_POINT ( 'NONE',  ( 93.99999999999985789, 268.4896896257338312, -84.99999999999997158 ) ) ;
#24407 = LINE ( 'NONE', #24843, #2192 ) ;
#24408 = CARTESIAN_POINT ( 'NONE',  ( 157.4999999999998579, 166.0806873385985796, -45.00000000000000000 ) ) ;
#24409 = ADVANCED_FACE ( 'NONE', ( #5996 ), #14772, .F. ) ;
#24410 = AXIS2_PLACEMENT_3D ( 'NONE', #12940, #2424, #25994 ) ;
#24411 = CARTESIAN_POINT ( 'NONE',  ( 9.345921402568903247, 140.0000000000000000, 14.99999999999999467 ) ) ;
#24412 = DIRECTION ( 'NONE',  ( -1.000000000000000000, 0.000000000000000000, 0.000000000000000000 ) ) ;
#24413 = LINE ( 'NONE', #26557, #3714 ) ;
#24414 = FACE_OUTER_BOUND ( 'NONE', #19867, .T. ) ;
#24415 = VECTOR ( 'NONE', #20112, 1000.000000000000114 ) ;
#24417 = EDGE_LOOP ( 'NONE', ( #27234, #6016, #24141, #16552 ) ) ;
#24416 = VERTEX_POINT ( 'NONE', #3412 ) ;
#24418 = AXIS2_PLACEMENT_3D ( 'NONE', #11962, #1027, #18975 ) ;
#24419 = CARTESIAN_POINT ( 'NONE',  ( -211.1098990695232374, 87.67290574086477761, -24.45168726860073605 ) ) ;
#24420 = AXIS2_PLACEMENT_3D ( 'NONE', #10432, #1937, #5832 ) ;
#24421 = DIRECTION ( 'NONE',  ( 1.000000000000000000, -0.000000000000000000, -0.000000000000000000 ) ) ;
#24422 = CARTESIAN_POINT ( 'NONE',  ( -206.8748453633142219, 90.47121226081961254, -26.13154464733097981 ) ) ;
#24423 = VERTEX_POINT ( 'NONE', #23247 ) ;
#24424 = ITEM_DEFINED_TRANSFORMATION ( 'NONE', 'NONE', #27594,  #10637 ) ;
#24425 = ORIENTED_EDGE ( 'NONE', *, *, #25234, .F. ) ;
#24426 = ORIENTED_EDGE ( 'NONE', *, *, #448, .T. ) ;
#24427 = DIRECTION ( 'NONE',  ( 1.000000000000000000, 0.000000000000000000, 0.000000000000000000 ) ) ;
#24428 = CARTESIAN_POINT ( 'NONE',  ( -149.3148642887314850, 125.0486274829139717, 18.95245273128049490 ) ) ;
#24429 = ORIENTED_EDGE ( 'NONE', *, *, #25406, .T. ) ;
#24430 = ORIENTED_EDGE ( 'NONE', *, *, #10922, .T. ) ;
#24431 = CIRCLE ( 'NONE', #22613, 7.499999999999992895 ) ;
#24432 = LINE ( 'NONE', #27010, #334 ) ;
#24433 = EDGE_CURVE ( 'NONE', #9062, #27691, #17057, .T. ) ;
#24434 = AXIS2_PLACEMENT_3D ( 'NONE', #23995, #10780, #8762 ) ;
#24435 = DIRECTION ( 'NONE',  ( 0.8916010070293584056, -0.4528218681382712996, 0.000000000000000000 ) ) ;
#24436 = EDGE_LOOP ( 'NONE', ( #21868, #13374, #2362, #13815 ) ) ;
#24437 = CARTESIAN_POINT ( 'NONE',  ( -204.4606010538157079, 92.01149164604352393, 28.73671646131870361 ) ) ;
#24438 = VECTOR ( 'NONE', #21228, 1000.000000000000114 ) ;
#24439 = DIRECTION ( 'NONE',  ( -0.000000000000000000, -0.000000000000000000, -1.000000000000000000 ) ) ;
#24440 = AXIS2_PLACEMENT_3D ( 'NONE', #8100, #6219, #19016 ) ;
#24441 = DIRECTION ( 'NONE',  ( 0.000000000000000000, 0.000000000000000000, 1.000000000000000000 ) ) ;
#24442 = CARTESIAN_POINT ( 'NONE',  ( -212.2468527728169931, 60.00277588997245459, -15.59298365947654297 ) ) ;
#24443 = ORIENTED_EDGE ( 'NONE', *, *, #28312, .F. ) ;
#24444 = EDGE_CURVE ( 'NONE', #23655, #8985, #1404, .T. ) ;
#24445 = EDGE_CURVE ( 'NONE', #10608, #6070, #17229, .T. ) ;
#24446 = FACE_OUTER_BOUND ( 'NONE', #12157, .T. ) ;
#24447 = CARTESIAN_POINT ( 'NONE',  ( -222.2072112174627136, 138.1987073436359026, -14.97424725141360291 ) ) ;
#24448 = DIRECTION ( 'NONE',  ( -0.000000000000000000, -0.000000000000000000, -1.000000000000000000 ) ) ;
#24449 = DIRECTION ( 'NONE',  ( 0.5555587585212703461, 0.8314772792026879911, -0.000000000000000000 ) ) ;
#24450 = VERTEX_POINT ( 'NONE', #12905 ) ;
#24451 = AXIS2_PLACEMENT_3D ( 'NONE', #9952, #7661, #7796 ) ;
#24452 = CARTESIAN_POINT ( 'NONE',  ( -260.0000000000001137, -165.0000000000001137, 60.00000000000002132 ) ) ;
#24453 = CIRCLE ( 'NONE', #28107, 19.07743405327024888 ) ;
#24454 = DIRECTION ( 'NONE',  ( 1.000000000000000000, 0.000000000000000000, 0.000000000000000000 ) ) ;
#24455 = DIRECTION ( 'NONE',  ( -0.000000000000000000, -0.000000000000000000, -1.000000000000000000 ) ) ;
#24456 = EDGE_LOOP ( 'NONE', ( #25690, #14333, #10272, #2693 ) ) ;
#24457 = CIRCLE ( 'NONE', #27221, 23.59849023212046149 ) ;
#24458 = ORIENTED_EDGE ( 'NONE', *, *, #22007, .F. ) ;
#24459 = EDGE_CURVE ( 'NONE', #23572, #17489, #28243, .T. ) ;
#24460 = AXIS2_PLACEMENT_3D ( 'NONE', #7437, #5129, #5409 ) ;
#24461 = EDGE_CURVE ( 'NONE', #3789, #8411, #13188, .T. ) ;
#24462 = DIRECTION ( 'NONE',  ( 0.000000000000000000, 0.000000000000000000, -1.000000000000000000 ) ) ;
#24463 = CARTESIAN_POINT ( 'NONE',  ( -203.1779787704217313, 93.05164332230199875, -28.77272332722132120 ) ) ;
#24464 = VERTEX_POINT ( 'NONE', #17335 ) ;
#24465 = ORIENTED_EDGE ( 'NONE', *, *, #20568, .F. ) ;
#24466 = CARTESIAN_POINT ( 'NONE',  ( 111.5363082892543218, -5.992022692082500157, 45.00000000000000000 ) ) ;
#24467 = FACE_OUTER_BOUND ( 'NONE', #7817, .T. ) ;
#24468 = VERTEX_POINT ( 'NONE', #19498 ) ;
#24469 = VERTEX_POINT ( 'NONE', #248 ) ;
#24470 = AXIS2_PLACEMENT_3D ( 'NONE', #4324, #6482, #22284 ) ;
#24471 = CARTESIAN_POINT ( 'NONE',  ( 28.57744295357075259, -14.51376905457599342, 45.00000000000000000 ) ) ;
#24472 = TOROIDAL_SURFACE ( 'NONE', #24005, -538.1631314933625845, 562.1290781602207289 ) ;
#24473 = PLANE ( 'NONE',  #24575 ) ;
#24474 = CARTESIAN_POINT ( 'NONE',  ( 158.0000000000006537, 143.2558747672816821, 45.00000000000000000 ) ) ;
#24475 = FACE_OUTER_BOUND ( 'NONE', #28045, .T. ) ;
#24476 = VECTOR ( 'NONE', #11991, 1000.000000000000000 ) ;
#24477 = FACE_OUTER_BOUND ( 'NONE', #21668, .T. ) ;
#24478 = CARTESIAN_POINT ( 'NONE',  ( -208.0819832607409410, 73.72223769926478099, -42.22193701883060868 ) ) ;
#24479 = DIRECTION ( 'NONE',  ( 0.000000000000000000, 0.000000000000000000, -1.000000000000000000 ) ) ;
#24480 = ORIENTED_EDGE ( 'NONE', *, *, #16314, .T. ) ;
#24481 = ADVANCED_FACE ( 'NONE', ( #21651 ), #24099, .F. ) ;
#24482 = CARTESIAN_POINT ( 'NONE',  ( 158.0000000000015916, 55.48024950453520177, 45.00000000000000000 ) ) ;
#24483 = LINE ( 'NONE', #19603, #7882 ) ;
#24484 = CARTESIAN_POINT ( 'NONE',  ( 134.9999999999998579, -150.0000000000000284, 84.99999999999995737 ) ) ;
#24485 = DIRECTION ( 'NONE',  ( -0.000000000000000000, -0.000000000000000000, -1.000000000000000000 ) ) ;
#24486 = ORIENTED_EDGE ( 'NONE', *, *, #8149, .T. ) ;
#24487 = CARTESIAN_POINT ( 'NONE',  ( 157.9999999999999716, 210.9684999699701393, -45.00000000000000000 ) ) ;
#24488 = VERTEX_POINT ( 'NONE', #10744 ) ;
#24489 = DIRECTION ( 'NONE',  ( 1.000000000000000000, 0.000000000000000000, 0.000000000000000000 ) ) ;
#24490 = CARTESIAN_POINT ( 'NONE',  ( -226.5998460896584561, 62.96930358458838128, -8.263950894743111064 ) ) ;
#24491 = CARTESIAN_POINT ( 'NONE',  ( 135.7881857370864225, 249.9921081881951750, -150.9608879355639885 ) ) ;
#24492 = ORIENTED_EDGE ( 'NONE', *, *, #10100, .T. ) ;
#24493 = PLANE ( 'NONE',  #1885 ) ;
#24494 = SURFACE_STYLE_FILL_AREA ( #8982 ) ;
#24495 = ORIENTED_EDGE ( 'NONE', *, *, #4234, .F. ) ;
#24496 = AXIS2_PLACEMENT_3D ( 'NONE', #7309, #5145, #976 ) ;
#24497 = CARTESIAN_POINT ( 'NONE',  ( -229.8570707599101297, 74.77602913581384314, 16.24303275925431933 ) ) ;
#24498 = ORIENTED_EDGE ( 'NONE', *, *, #14243, .F. ) ;
#24499 = CARTESIAN_POINT ( 'NONE',  ( -175.0000000000000000, -120.0000000000001847, -76.02499999999999147 ) ) ;
#24500 = ORIENTED_EDGE ( 'NONE', *, *, #9628, .F. ) ;
#24501 = AXIS2_PLACEMENT_3D ( 'NONE', #5044, #3165, #11954 ) ;
#24502 = ADVANCED_FACE ( 'NONE', ( #6423 ), #3436, .T. ) ;
#24503 = ORIENTED_EDGE ( 'NONE', *, *, #2460, .F. ) ;
#24504 = EDGE_CURVE ( 'NONE', #2475, #8983, #17476, .T. ) ;
#24505 = LINE ( 'NONE', #4811, #10402 ) ;
#24506 = ORIENTED_EDGE ( 'NONE', *, *, #9614, .T. ) ;
#24507 = EDGE_CURVE ( 'NONE', #23616, #15078, #22218, .T. ) ;
#24508 = EDGE_LOOP ( 'NONE', ( #4746, #12674, #25382, #14786 ) ) ;
#24509 = ORIENTED_EDGE ( 'NONE', *, *, #6690, .T. ) ;
#24510 = CARTESIAN_POINT ( 'NONE',  ( 105.5907556405553720, 242.1385898947461328, 29.32397797499837466 ) ) ;
#24511 = CARTESIAN_POINT ( 'NONE',  ( 340.3127869742386338, 101.4626071723496779, -137.4901433416540328 ) ) ;
#24512 = CARTESIAN_POINT ( 'NONE',  ( -221.1044245926312044, 138.9463871349868782, -14.97905406095859249 ) ) ;
#24513 = AXIS2_PLACEMENT_3D ( 'NONE', #15545, #17977, #2739 ) ;
#24514 = DIRECTION ( 'NONE',  ( -1.000000000000000000, -0.000000000000000000, -2.775557561562887407E-16 ) ) ;
#24515 = CARTESIAN_POINT ( 'NONE',  ( -160.0000000000000284, 59.99999999999994316, 15.00000000000000000 ) ) ;
#24516 = DIRECTION ( 'NONE',  ( -0.8916010070296327417, -0.4528218681377311761, 0.000000000000000000 ) ) ;
#24517 = CARTESIAN_POINT ( 'NONE',  ( 1.633516369018864323, -1.249999999999998890, -7.514731128045609942 ) ) ;
#24518 = CARTESIAN_POINT ( 'NONE',  ( 157.9999999999997442, 251.6023750975910218, 45.00000000000000000 ) ) ;
#24519 = VECTOR ( 'NONE', #25600, 1000.000000000000000 ) ;
#24520 = CARTESIAN_POINT ( 'NONE',  ( 158.0000000000009663, 111.1613746771971876, -45.00000000000000000 ) ) ;
#24521 = CARTESIAN_POINT ( 'NONE',  ( 65.00000000000000000, -150.0000000000000568, 70.00000000000001421 ) ) ;
#24522 = LINE ( 'NONE', #17628, #17112 ) ;
#24523 = ORIENTED_EDGE ( 'NONE', *, *, #13251, .F. ) ;
#24524 = DIRECTION ( 'NONE',  ( 0.000000000000000000, 9.251858538542967883E-17, -1.000000000000000000 ) ) ;
#24525 = CARTESIAN_POINT ( 'NONE',  ( 157.4999999999995168, 208.7145624662163925, 45.00000000000000000 ) ) ;
#24526 = DIRECTION ( 'NONE',  ( 1.000000000000000000, 0.000000000000000000, -0.000000000000000000 ) ) ;
#24527 = CARTESIAN_POINT ( 'NONE',  ( -28.05246235954390244, 188.0718642840173516, 15.00000000000000000 ) ) ;
#24528 = ORIENTED_EDGE ( 'NONE', *, *, #24096, .T. ) ;
#24529 = CARTESIAN_POINT ( 'NONE',  ( 109.9639884629222877, 258.5863491989132967, -43.28603914697800548 ) ) ;
#24530 = VERTEX_POINT ( 'NONE', #15625 ) ;
#24531 = DIRECTION ( 'NONE',  ( 0.000000000000000000, 0.000000000000000000, 1.000000000000000000 ) ) ;
#24532 = EDGE_CURVE ( 'NONE', #8917, #26858, #21932, .T. ) ;
#24533 = AXIS2_PLACEMENT_3D ( 'NONE', #4005, #10064, #23275 ) ;
#24534 = ORIENTED_EDGE ( 'NONE', *, *, #10319, .T. ) ;
#24535 = EDGE_CURVE ( 'NONE', #7370, #23432, #9006, .T. ) ;
#24536 = EDGE_CURVE ( 'NONE', #28324, #23545, #19510, .T. ) ;
#24537 = ORIENTED_EDGE ( 'NONE', *, *, #26992, .F. ) ;
#24538 = ORIENTED_EDGE ( 'NONE', *, *, #28077, .F. ) ;
#24539 = VECTOR ( 'NONE', #10430, 1000.000000000000000 ) ;
#24540 = ORIENTED_EDGE ( 'NONE', *, *, #8298, .F. ) ;
#24541 = CARTESIAN_POINT ( 'NONE',  ( 119.9999999999998863, 330.0000000000000000, -90.00000000000004263 ) ) ;
#24542 = CARTESIAN_POINT ( 'NONE',  ( -210.0000000000000568, 30.00000000000080647, 79.99999999999889155 ) ) ;
#24543 = LINE ( 'NONE', #10653, #23061 ) ;
#24544 = DIRECTION ( 'NONE',  ( 1.000000000000000000, 0.000000000000000000, -0.000000000000000000 ) ) ;
#24545 = CARTESIAN_POINT ( 'NONE',  ( 267.4999999999996021, 194.4107529906318348, 75.35061095560300259 ) ) ;
#24546 = CARTESIAN_POINT ( 'NONE',  ( -220.5757601432209185, 60.53190028572070958, 22.93231238515498305 ) ) ;
#24547 = LINE ( 'NONE', #4856, #9587 ) ;
#24548 = FACE_OUTER_BOUND ( 'NONE', #5362, .T. ) ;
#24549 = DIRECTION ( 'NONE',  ( -0.000000000000000000, 0.000000000000000000, -1.000000000000000000 ) ) ;
#24550 = AXIS2_PLACEMENT_3D ( 'NONE', #9991, #3372, #3794 ) ;
#24551 = CARTESIAN_POINT ( 'NONE',  ( -219.7365213294408477, 87.93330934136336907, -16.54735205736179893 ) ) ;
#24552 = DIRECTION ( 'NONE',  ( 0.000000000000000000, -1.000000000000000000, 0.000000000000000000 ) ) ;
#24553 = CARTESIAN_POINT ( 'NONE',  ( 158.0000000000006537, 143.7637497747887210, -45.00000000000000000 ) ) ;
#24554 = VECTOR ( 'NONE', #13323, 1000.000000000000000 ) ;
#24555 = PLANE ( 'NONE',  #17087 ) ;
#24556 = CIRCLE ( 'NONE', #9900, 10.71881775658151170 ) ;
#24557 = CARTESIAN_POINT ( 'NONE',  ( -1.097484912870223539, 135.6466149407013688, 15.26443675455116455 ) ) ;
#24558 = PLANE ( 'NONE',  #1352 ) ;
#24559 = DIRECTION ( 'NONE',  ( -0.8916010070293682865, -0.4528218681382519262, 0.000000000000000000 ) ) ;
#24560 = DIRECTION ( 'NONE',  ( 0.8660254037844432595, 0.4999999999999919509, -0.000000000000000000 ) ) ;
#24561 = CIRCLE ( 'NONE', #24092, 1.999999999999990452 ) ;
#24563 = ORIENTED_EDGE ( 'NONE', *, *, #21511, .F. ) ;
#24562 = VERTEX_POINT ( 'NONE', #2241 ) ;
#24564 = FACE_OUTER_BOUND ( 'NONE', #22229, .T. ) ;
#24565 = EDGE_CURVE ( 'NONE', #17857, #13481, #17761, .T. ) ;
#24566 = CARTESIAN_POINT ( 'NONE',  ( 157.9999999999999716, 210.9684999699701393, -45.00000000000000000 ) ) ;
#24567 = ORIENTED_EDGE ( 'NONE', *, *, #6660, .T. ) ;
#24568 = ORIENTED_EDGE ( 'NONE', *, *, #3892, .T. ) ;
#24569 = ORIENTED_EDGE ( 'NONE', *, *, #7156, .T. ) ;
#24570 = EDGE_CURVE ( 'NONE', #3147, #25123, #10795, .T. ) ;
#24571 = DIRECTION ( 'NONE',  ( 0.7071067811867438602, 8.659560562352529298E-17, 0.7071067811863512853 ) ) ;
#24572 = CARTESIAN_POINT ( 'NONE',  ( -122.8162676995331708, 132.7862067426565886, 15.82969067823930587 ) ) ;
#24573 = EDGE_CURVE ( 'NONE', #13590, #2802, #22076, .T. ) ;
#24574 = ORIENTED_EDGE ( 'NONE', *, *, #486, .F. ) ;
#24575 = AXIS2_PLACEMENT_3D ( 'NONE', #11562, #633, #24763 ) ;
#24576 = ORIENTED_EDGE ( 'NONE', *, *, #13984, .T. ) ;
#24577 = AXIS2_PLACEMENT_3D ( 'NONE', #27443, #21131, #3598 ) ;
#24578 = LINE ( 'NONE', #7200, #20050 ) ;
#24579 = CARTESIAN_POINT ( 'NONE',  ( 157.4999999999998579, 100.8759371434154701, -45.00000000000000000 ) ) ;
#24580 = VERTEX_POINT ( 'NONE', #15485 ) ;
#24581 = DIRECTION ( 'NONE',  ( -0.000000000000000000, -0.000000000000000000, -1.000000000000000000 ) ) ;
#24582 = VECTOR ( 'NONE', #25295, 1000.000000000000000 ) ;
#24583 = LINE ( 'NONE', #16116, #15322 ) ;
#24584 = CARTESIAN_POINT ( 'NONE',  ( -49.97791255360778706, 113.2029523930418975, -145.0000000000000000 ) ) ;
#24585 = LINE ( 'NONE', #13683, #22374 ) ;
#24586 = CARTESIAN_POINT ( 'NONE',  ( -210.0090741174316804, 73.93180346605655018, -34.41452853221989727 ) ) ;
#24587 = ORIENTED_EDGE ( 'NONE', *, *, #14550, .F. ) ;
#24588 = DIRECTION ( 'NONE',  ( 0.000000000000000000, -1.000000000000000000, 0.000000000000000000 ) ) ;
#24589 = CIRCLE ( 'NONE', #22749, 10.53396790234564762 ) ;
#24590 = ADVANCED_FACE ( 'NONE', ( #19773 ), #23652, .F. ) ;
#24591 = CARTESIAN_POINT ( 'NONE',  ( -217.7401460507702780, 138.5677444271782122, -12.99353264123096885 ) ) ;
#24592 = CARTESIAN_POINT ( 'NONE',  ( 157.9999999999997726, 244.0787500750700474, 45.00000000000000000 ) ) ;
#24593 = LINE ( 'NONE', #20132, #7554 ) ;
#24594 = ORIENTED_EDGE ( 'NONE', *, *, #15688, .F. ) ;
#24595 = VECTOR ( 'NONE', #7650, 1000.000000000000114 ) ;
#24596 = CARTESIAN_POINT ( 'NONE',  ( -63.57415822541634043, 80.97823757117562593, 100.0000000000000000 ) ) ;
#24597 = EDGE_CURVE ( 'NONE', #7010, #4812, #23813, .T. ) ;
#24598 = CARTESIAN_POINT ( 'NONE',  ( -227.3197243376772860, 73.27520359174637576, 17.23934621637404163 ) ) ;
#24599 = CARTESIAN_POINT ( 'NONE',  ( 157.9999999999997726, 248.5866250825770294, -45.00000000000000000 ) ) ;
#24600 = ORIENTED_EDGE ( 'NONE', *, *, #7483, .F. ) ;
#24601 =( NAMED_UNIT ( * ) SI_UNIT ( $, .STERADIAN. ) SOLID_ANGLE_UNIT ( ) );
#24602 = CONICAL_SURFACE ( 'NONE', #738, 6.000000000000005329, 1.029744258676651647 ) ;
#24603 = EDGE_LOOP ( 'NONE', ( #7446, #18705, #27726, #2913, #8769, #14836, #8763, #3859, #5168, #24632 ) ) ;
#24604 = CARTESIAN_POINT ( 'NONE',  ( 90.92319367352486381, 112.0484670279021771, 72.65625000014701129 ) ) ;
#24605 = CARTESIAN_POINT ( 'NONE',  ( 158.0000000000000568, 203.4448749474510407, -45.00000000000000000 ) ) ;
#24606 = EDGE_CURVE ( 'NONE', #378, #7332, #26239, .T. ) ;
#24607 = ORIENTED_EDGE ( 'NONE', *, *, #7624, .T. ) ;
#24608 = VERTEX_POINT ( 'NONE', #4539 ) ;
#24609 = DIRECTION ( 'NONE',  ( 0.000000000000000000, 0.000000000000000000, 1.000000000000000000 ) ) ;
#24610 = ADVANCED_FACE ( 'NONE', ( #13327 ), #20490, .F. ) ;
#24611 = CARTESIAN_POINT ( 'NONE',  ( 157.4999999999995737, 203.6988124512014338, 45.00000000000000000 ) ) ;
#24612 = ORIENTED_EDGE ( 'NONE', *, *, #4213, .T. ) ;
#24613 = LINE ( 'NONE', #2767, #17396 ) ;
#24614 = ORIENTED_EDGE ( 'NONE', *, *, #17829, .F. ) ;
#24615 = AXIS2_PLACEMENT_3D ( 'NONE', #19195, #27940, #19336 ) ;
#24616 = FACE_BOUND ( 'NONE', #9203, .T. ) ;
#24617 = CARTESIAN_POINT ( 'NONE',  ( -175.0000000000000000, -170.0000000000001705, 76.00000000000000000 ) ) ;
#24618 = CARTESIAN_POINT ( 'NONE',  ( 157.4999999999998579, 83.32081209086616980, 45.00000000000000000 ) ) ;
#24619 = CARTESIAN_POINT ( 'NONE',  ( -20.28198206961980787, 129.6360743166005705, -16.81503550425660265 ) ) ;
#24620 = VECTOR ( 'NONE', #3378, 1000.000000000000000 ) ;
#24621 = LINE ( 'NONE', #16013, #8196 ) ;
#24622 = EDGE_CURVE ( 'NONE', #3041, #21312, #27093, .T. ) ;
#24623 = CARTESIAN_POINT ( 'NONE',  ( 158.0000000000007390, 133.7322497447605656, 45.00000000000000000 ) ) ;
#24624 = CARTESIAN_POINT ( 'NONE',  ( 158.0000000000012790, 85.57474959461971764, 45.00000000000000000 ) ) ;
#24625 = ORIENTED_EDGE ( 'NONE', *, *, #3111, .F. ) ;
#24626 = LINE ( 'NONE', #2779, #25136 ) ;
#24627 = CARTESIAN_POINT ( 'NONE',  ( -223.3099978423093432, 137.4510275522739562, 14.96944044186858491 ) ) ;
#24628 = CARTESIAN_POINT ( 'NONE',  ( 9.999999999999749534, 90.00000000000001421, 110.0000000000000284 ) ) ;
#24629 = CARTESIAN_POINT ( 'NONE',  ( -248.1546605714623013, -91.18033988749901653, -16.91094714394370158 ) ) ;
#24630 = ORIENTED_EDGE ( 'NONE', *, *, #25986, .T. ) ;
#24631 = CARTESIAN_POINT ( 'NONE',  ( -229.6839157287631963, 64.28192771017235430, 7.255073467994254344 ) ) ;
#24632 = ORIENTED_EDGE ( 'NONE', *, *, #17358, .T. ) ;
#24633 = EDGE_CURVE ( 'NONE', #543, #6469, #11752, .T. ) ;
#24634 = LINE ( 'NONE', #216, #19403 ) ;
#24635 = DIRECTION ( 'NONE',  ( -1.000000000000000000, 0.000000000000000000, 0.000000000000000000 ) ) ;
#24636 = DIRECTION ( 'NONE',  ( -0.5790253867566403922, -0.8153095126952237814, -0.000000000000000000 ) ) ;
#24637 = VERTEX_POINT ( 'NONE', #531 ) ;
#24638 = CARTESIAN_POINT ( 'NONE',  ( 157.4999999999998579, 78.30506207585207790, 45.00000000000000000 ) ) ;
#24639 = LINE ( 'NONE', #22773, #8831 ) ;
#24640 = ORIENTED_EDGE ( 'NONE', *, *, #14586, .F. ) ;
#24641 = VECTOR ( 'NONE', #16180, 1000.000000000000000 ) ;
#24642 = DIRECTION ( 'NONE',  ( 0.8916010070295005141, -0.4528218681379915789, 0.000000000000000000 ) ) ;
#24643 = ORIENTED_EDGE ( 'NONE', *, *, #3709, .T. ) ;
#24644 = DIRECTION ( 'NONE',  ( -0.000000000000000000, -0.000000000000000000, -1.000000000000000000 ) ) ;
#24645 = ORIENTED_EDGE ( 'NONE', *, *, #14238, .F. ) ;
#24646 = ORIENTED_EDGE ( 'NONE', *, *, #10137, .T. ) ;
#24647 = ADVANCED_FACE ( 'NONE', ( #7424 ), #6988, .F. ) ;
#24648 = LINE ( 'NONE', #12007, #3971 ) ;
#24649 = EDGE_LOOP ( 'NONE', ( #8425, #18744, #14829, #10188 ) ) ;
#24650 = EDGE_CURVE ( 'NONE', #553, #14507, #18608, .T. ) ;
#24651 = ORIENTED_EDGE ( 'NONE', *, *, #17172, .F. ) ;
#24652 = ORIENTED_EDGE ( 'NONE', *, *, #4570, .T. ) ;
#24653 = CARTESIAN_POINT ( 'NONE',  ( 105.7413873646089684, 247.3652972445288469, 29.41146778675347662 ) ) ;
#24654 = CARTESIAN_POINT ( 'NONE',  ( 158.0000000000003411, 175.8582498648732440, -45.00000000000000000 ) ) ;
#24655 = CARTESIAN_POINT ( 'NONE',  ( -225.3736415174282115, 135.7651958811247539, -14.97905406095859604 ) ) ;
#24656 = VECTOR ( 'NONE', #7051, 1000.000000000000000 ) ;
#24657 = EDGE_CURVE ( 'NONE', #11940, #4647, #9294, .T. ) ;
#24658 = CARTESIAN_POINT ( 'NONE',  ( 158.0000000000006537, 145.7637497747887210, 45.00000000000000000 ) ) ;
#24659 = DIRECTION ( 'NONE',  ( -1.000000000000000000, 0.000000000000000000, 0.000000000000000000 ) ) ;
#24660 = LINE ( 'NONE', #3092, #9287 ) ;
#24661 = CYLINDRICAL_SURFACE ( 'NONE', #755, 22.49999999999999289 ) ;
#24662 = CARTESIAN_POINT ( 'NONE',  ( 65.00000000000000000, -120.0000000000000711, 76.02500000000001990 ) ) ;
#24663 = CARTESIAN_POINT ( 'NONE',  ( 157.4999999999998579, 176.1121873686267350, 45.00000000000000000 ) ) ;
#24664 = PLANE ( 'NONE',  #843 ) ;
#24665 = DIRECTION ( 'NONE',  ( 0.000000000000000000, -1.000000000000000000, 0.000000000000000000 ) ) ;
#24666 = VERTEX_POINT ( 'NONE', #24518 ) ;
#24667 = CARTESIAN_POINT ( 'NONE',  ( 319.9779125536060178, 113.2029523930392969, -145.0000000000000000 ) ) ;
#24668 = EDGE_CURVE ( 'NONE', #26578, #25616, #16198, .T. ) ;
#24669 = PLANE ( 'NONE',  #26581 ) ;
#24670 = CARTESIAN_POINT ( 'NONE',  ( 197.6424708188942816, 64.50455043276784295, 45.00000000000000000 ) ) ;
#24671 = EDGE_CURVE ( 'NONE', #28009, #3903, #2961, .T. ) ;
#24672 = CARTESIAN_POINT ( 'NONE',  ( 106.9638955565933145, 209.3217385430746447, -141.3400049877799916 ) ) ;
#24673 = VERTEX_POINT ( 'NONE', #26954 ) ;
#24674 = AXIS2_PLACEMENT_3D ( 'NONE', #1329, #10240, #18998 ) ;
#24675 = CARTESIAN_POINT ( 'NONE',  ( 157.4999999999996874, 271.4114376538935289, 45.00000000000000000 ) ) ;
#24676 = ORIENTED_EDGE ( 'NONE', *, *, #21926, .T. ) ;
#24677 = CARTESIAN_POINT ( 'NONE',  ( 179.9999999999999147, 526.4263741777961059, 100.0000000000000142 ) ) ;
#24678 = VECTOR ( 'NONE', #13929, 999.9999999999998863 ) ;
#24679 = ORIENTED_EDGE ( 'NONE', *, *, #3438, .T. ) ;
#24680 = ORIENTED_EDGE ( 'NONE', *, *, #12229, .F. ) ;
#24681 = EDGE_CURVE ( 'NONE', #27184, #1982, #389, .T. ) ;
#24682 = ORIENTED_EDGE ( 'NONE', *, *, #25300, .F. ) ;
#24683 = ORIENTED_EDGE ( 'NONE', *, *, #9189, .T. ) ;
#24684 = CARTESIAN_POINT ( 'NONE',  ( -62.44394432210693680, 134.9077315552440837, 13.78060465110143262 ) ) ;
#24685 = DIRECTION ( 'NONE',  ( -0.000000000000000000, 1.000000000000000000, -1.387778780781445429E-16 ) ) ;
#24686 = DIRECTION ( 'NONE',  ( 0.000000000000000000, 1.214306433183764966E-16, -1.000000000000000000 ) ) ;
#24687 = LINE ( 'NONE', #23100, #25225 ) ;
#24688 = PRODUCT_DEFINITION_CONTEXT ( 'detailed design', #23235, 'design' ) ;
#24689 = FACE_OUTER_BOUND ( 'NONE', #22433, .T. ) ;
#24690 = CARTESIAN_POINT ( 'NONE',  ( -222.1843861435932581, 71.54148064075766911, 20.10873357379271908 ) ) ;
#24692 = FACE_OUTER_BOUND ( 'NONE', #2020, .T. ) ;
#24691 = AXIS2_PLACEMENT_3D ( 'NONE', #8017, #16644, #25258 ) ;
#24693 = FACE_OUTER_BOUND ( 'NONE', #2027, .T. ) ;
#24694 = CARTESIAN_POINT ( 'NONE',  ( 79.99999999999995737, 102.6016043537709379, -89.82480251742194355 ) ) ;
#24695 = AXIS2_PLACEMENT_3D ( 'NONE', #1747, #21008, #8085 ) ;
#24696 = CARTESIAN_POINT ( 'NONE',  ( -214.0809518536805172, 88.01152685125013875, -20.18792008739580268 ) ) ;
#24697 = LINE ( 'NONE', #1886, #8767 ) ;
#24698 = CARTESIAN_POINT ( 'NONE',  ( 158.0000000000008527, 123.7007497147323960, -45.00000000000000000 ) ) ;
#24699 = DIRECTION ( 'NONE',  ( 0.000000000000000000, 1.000000000000000000, 0.000000000000000000 ) ) ;
#24700 = EDGE_CURVE ( 'NONE', #20571, #5309, #24556, .T. ) ;
#24701 = EDGE_CURVE ( 'NONE', #14569, #20039, #2063, .T. ) ;
#24702 = APPLICATION_CONTEXT ( 'automotive_design' ) ;
#24703 = CARTESIAN_POINT ( 'NONE',  ( 5.596985676125543208, 137.4248447260847854, 15.08939176349822020 ) ) ;
#24704 = FACE_OUTER_BOUND ( 'NONE', #12498, .T. ) ;
#24705 = DIRECTION ( 'NONE',  ( -0.8916010070298151513, 0.4528218681373720744, 0.000000000000000000 ) ) ;
#24706 = CARTESIAN_POINT ( 'NONE',  ( 232.4999999999996305, 194.4107529906318064, 288.0938197134494203 ) ) ;
#24708 = ORIENTED_EDGE ( 'NONE', *, *, #12321, .F. ) ;
#24707 = ORIENTED_EDGE ( 'NONE', *, *, #9979, .T. ) ;
#24709 = DIRECTION ( 'NONE',  ( 0.000000000000000000, 0.000000000000000000, -1.000000000000000000 ) ) ;
#24710 = PLANE ( 'NONE',  #14343 ) ;
#24711 = ORIENTED_EDGE ( 'NONE', *, *, #7442, .T. ) ;
#24712 = ORIENTED_EDGE ( 'NONE', *, *, #14332, .T. ) ;
#24713 = ORIENTED_EDGE ( 'NONE', *, *, #7052, .T. ) ;
#24714 = CIRCLE ( 'NONE', #23787, 30.00000000000002842 ) ;
#24715 = LINE ( 'NONE', #7046, #117 ) ;
#24716 = CARTESIAN_POINT ( 'NONE',  ( -142.3006454101396514, 127.5200935965802387, 17.68125478821149699 ) ) ;
#24717 = EDGE_CURVE ( 'NONE', #20004, #2614, #11463, .T. ) ;
#24718 = CIRCLE ( 'NONE', #24256, 7.499999999999992895 ) ;
#24719 = EDGE_LOOP ( 'NONE', ( #20467, #19727, #3204 ) ) ;
#24720 = ORIENTED_EDGE ( 'NONE', *, *, #20516, .T. ) ;
#24721 = CARTESIAN_POINT ( 'NONE',  ( 2.399999999999999911, 1.249999999999999556, -7.582700855991164168 ) ) ;
#24722 = CARTESIAN_POINT ( 'NONE',  ( 134.9999999999998579, 250.0000000000000568, -138.9999999999999432 ) ) ;
#24723 = ADVANCED_FACE ( 'NONE', ( #4967 ), #18142, .T. ) ;
#24724 = CARTESIAN_POINT ( 'NONE',  ( 158.0000000000001705, 188.9054999099155054, 45.00000000000000000 ) ) ;
#24725 = ORIENTED_EDGE ( 'NONE', *, *, #20136, .T. ) ;
#24726 = FILL_AREA_STYLE ('',( #18120 ) ) ;
#24727 = CARTESIAN_POINT ( 'NONE',  ( -17.24491960465746132, -23.01420295945612082, 100.0000000000000000 ) ) ;
#24728 = VECTOR ( 'NONE', #16262, 1000.000000000000000 ) ;
#24729 = DIRECTION ( 'NONE',  ( 0.000000000000000000, 9.251858538542967883E-17, -1.000000000000000000 ) ) ;
#24730 = ADVANCED_FACE ( 'NONE', ( #22796 ), #9444, .F. ) ;
#24731 = DIRECTION ( 'NONE',  ( -0.8916010070297440970, 0.4528218681375119625, 0.000000000000000000 ) ) ;
#24732 = CARTESIAN_POINT ( 'NONE',  ( -208.0231409554068875, 75.22252239880569391, -40.22632386312260167 ) ) ;
#24733 = ADVANCED_FACE ( 'NONE', ( #951 ), #9150, .F. ) ;
#24734 = AXIS2_PLACEMENT_3D ( 'NONE', #27568, #12516, #16954 ) ;
#24735 = DIRECTION ( 'NONE',  ( -0.8916010070299780210, -0.4528218681370510534, 0.000000000000000000 ) ) ;
#24736 = EDGE_CURVE ( 'NONE', #1342, #24933, #15399, .T. ) ;
#24737 = CIRCLE ( 'NONE', #12359, 5.000000000000004441 ) ;
#24738 = CARTESIAN_POINT ( 'NONE',  ( -220.9647007329185158, 136.4514858755404987, -12.97939780113087060 ) ) ;
#24739 = CARTESIAN_POINT ( 'NONE',  ( 157.4999999999998579, 133.4783122410070462, 45.00000000000000000 ) ) ;
#24740 = LINE ( 'NONE', #12100, #4777 ) ;
#24741 = ORIENTED_EDGE ( 'NONE', *, *, #18472, .T. ) ;
#24742 = VECTOR ( 'NONE', #4363, 1000.000000000000000 ) ;
#24743 = CARTESIAN_POINT ( 'NONE',  ( 134.9999999999998579, 220.0000000000000284, -189.9999999999999716 ) ) ;
#24744 = AXIS2_PLACEMENT_3D ( 'NONE', #23437, #12820, #12683 ) ;
#24745 = CYLINDRICAL_SURFACE ( 'NONE', #9351, 75.00000000000002842 ) ;
#24746 = CARTESIAN_POINT ( 'NONE',  ( 65.00000000000000000, -120.0000000000000711, 76.00000000000001421 ) ) ;
#24747 = VERTEX_POINT ( 'NONE', #3820 ) ;
#24748 = ORIENTED_EDGE ( 'NONE', *, *, #1174, .T. ) ;
#24749 = CARTESIAN_POINT ( 'NONE',  ( 107.3061218092289408, 127.3934823308085242, 87.81249999970602005 ) ) ;
#24750 = FACE_OUTER_BOUND ( 'NONE', #7509, .T. ) ;
#24751 = ORIENTED_EDGE ( 'NONE', *, *, #22068, .F. ) ;
#24752 = AXIS2_PLACEMENT_3D ( 'NONE', #24899, #7086, #7375 ) ;
#24753 = ORIENTED_EDGE ( 'NONE', *, *, #5069, .F. ) ;
#24754 = CARTESIAN_POINT ( 'NONE',  ( 157.4999999999998579, 98.36806213590843129, 45.00000000000000000 ) ) ;
#24755 = AXIS2_PLACEMENT_3D ( 'NONE', #14082, #22403, #3132 ) ;
#24756 = DIRECTION ( 'NONE',  ( 0.7071067811865474617, 8.659560562354932858E-17, 0.7071067811865474617 ) ) ;
#24757 = VERTEX_POINT ( 'NONE', #5555 ) ;
#24758 = CARTESIAN_POINT ( 'NONE',  ( 157.4999999999998295, 40.68693696324645970, -45.00000000000000000 ) ) ;
#24759 = ORIENTED_EDGE ( 'NONE', *, *, #14985, .T. ) ;
#24760 = DIRECTION ( 'NONE',  ( 0.8916010070293483025, 0.4528218681382912836, 0.000000000000000000 ) ) ;
#24761 = AXIS2_PLACEMENT_3D ( 'NONE', #22713, #25004, #27150 ) ;
#24762 = EDGE_CURVE ( 'NONE', #12951, #2873, #10157, .T. ) ;
#24763 = DIRECTION ( 'NONE',  ( -0.000000000000000000, 0.000000000000000000, -1.000000000000000000 ) ) ;
#24764 = DIRECTION ( 'NONE',  ( 1.000000000000000000, 0.000000000000000000, -0.000000000000000000 ) ) ;
#24765 = CARTESIAN_POINT ( 'NONE',  ( -13.80312808312014816, 130.8720850416648318, -14.97150579888662492 ) ) ;
#24766 = CARTESIAN_POINT ( 'NONE',  ( -110.3221550338875687, 20.24192588826928585, 83.00000000000001421 ) ) ;
#24767 = CARTESIAN_POINT ( 'NONE',  ( -264.4238960014317286, -166.0091389525178727, -89.67888693108041309 ) ) ;
#24768 = DIRECTION ( 'NONE',  ( 1.000000000000000000, 0.000000000000000000, 0.000000000000000000 ) ) ;
#24769 = VERTEX_POINT ( 'NONE', #12464 ) ;
#24770 = VECTOR ( 'NONE', #466, 1000.000000000000000 ) ;
#24771 = DIRECTION ( 'NONE',  ( -0.000000000000000000, 1.000000000000000000, -1.387778780781445429E-16 ) ) ;
#24772 = ADVANCED_FACE ( 'NONE', ( #17037 ), #5701, .F. ) ;
#24773 = PLANE ( 'NONE',  #23014 ) ;
#24774 = CARTESIAN_POINT ( 'NONE',  ( 157.4999999999998579, 158.5570623160774630, 45.00000000000000000 ) ) ;
#24775 = LINE ( 'NONE', #24914, #176 ) ;
#24776 = ORIENTED_EDGE ( 'NONE', *, *, #17648, .F. ) ;
#24777 = CARTESIAN_POINT ( 'NONE',  ( -239.7229382034103935, 70.94047833162915140, 5.249966640536482210 ) ) ;
#24778 = CIRCLE ( 'NONE', #22477, 2.000000000000000000 ) ;
#24779 = ORIENTED_EDGE ( 'NONE', *, *, #21129, .F. ) ;
#24780 = ADVANCED_FACE ( 'NONE', ( #18910 ), #8137, .F. ) ;
#24781 = DIRECTION ( 'NONE',  ( 0.000000000000000000, 0.000000000000000000, -1.000000000000000000 ) ) ;
#24782 = CARTESIAN_POINT ( 'NONE',  ( -17.24491960465747553, 80.97823757117562593, 80.00000000000001421 ) ) ;
#24783 = DIRECTION ( 'NONE',  ( 1.000000000000000000, 1.541976423090495387E-16, -0.000000000000000000 ) ) ;
#24784 = VERTEX_POINT ( 'NONE', #14607 ) ;
#24785 = DIRECTION ( 'NONE',  ( 0.000000000000000000, 0.000000000000000000, -1.000000000000000000 ) ) ;
#24786 = ORIENTED_EDGE ( 'NONE', *, *, #24823, .F. ) ;
#24787 = CARTESIAN_POINT ( 'NONE',  ( -47.90464318815075018, 130.8803359162888569, 16.39305836622124346 ) ) ;
#24788 = VERTEX_POINT ( 'NONE', #23089 ) ;
#24789 = LINE ( 'NONE', #9276, #18161 ) ;
#24790 = ORIENTED_EDGE ( 'NONE', *, *, #2274, .T. ) ;
#24791 = ORIENTED_EDGE ( 'NONE', *, *, #13729, .F. ) ;
#24792 = CARTESIAN_POINT ( 'NONE',  ( 158.0000000000017053, 45.44874947450702507, 45.00000000000000000 ) ) ;
#24793 = ORIENTED_EDGE ( 'NONE', *, *, #6497, .F. ) ;
#24794 = AXIS2_PLACEMENT_3D ( 'NONE', #11743, #18051, #5108 ) ;
#24795 = ORIENTED_EDGE ( 'NONE', *, *, #6193, .T. ) ;
#24796 = ORIENTED_EDGE ( 'NONE', *, *, #4655, .T. ) ;
#24797 = CARTESIAN_POINT ( 'NONE',  ( 115.5814157129578916, 232.3660254037840502, -45.00000000000000000 ) ) ;
#24798 = VECTOR ( 'NONE', #17084, 1000.000000000000000 ) ;
#24799 = EDGE_CURVE ( 'NONE', #10, #25897, #7605, .T. ) ;
#24800 = LINE ( 'NONE', #24654, #8038 ) ;
#24801 = CARTESIAN_POINT ( 'NONE',  ( 158.0000000000007390, 133.7322497447605656, 45.00000000000000000 ) ) ;
#24802 = CARTESIAN_POINT ( 'NONE',  ( 109.9999999999999005, 260.0000000000000000, -45.00000000000000000 ) ) ;
#24803 = CARTESIAN_POINT ( 'NONE',  ( -210.0000000000000568, -220.0000000000000853, 90.00000000000002842 ) ) ;
#24804 = FACE_OUTER_BOUND ( 'NONE', #2202, .T. ) ;
#24805 = CARTESIAN_POINT ( 'NONE',  ( 157.4999999999998579, 45.70268697826052318, -45.00000000000000000 ) ) ;
#24806 = CARTESIAN_POINT ( 'NONE',  ( -160.0000000000000284, 59.99999999999994316, -15.00000000000000000 ) ) ;
#24807 = CARTESIAN_POINT ( 'NONE',  ( -261.6154359210910911, -166.7250444216647054, 110.0000000000000142 ) ) ;
#24808 = CARTESIAN_POINT ( 'NONE',  ( -175.0000000000000000, -120.0000000000001705, 70.00000000000001421 ) ) ;
#24809 = CARTESIAN_POINT ( 'NONE',  ( 217.4999999999996305, 83.06687458711267880, 36.86484227207694175 ) ) ;
#24810 = EDGE_LOOP ( 'NONE', ( #4984, #26224, #10301, #25158 ) ) ;
#24811 = CARTESIAN_POINT ( 'NONE',  ( 158.0000000000017053, 43.44874947450702507, 45.00000000000000000 ) ) ;
#24812 = EDGE_CURVE ( 'NONE', #17465, #19653, #11271, .T. ) ;
#24813 = VECTOR ( 'NONE', #5109, 1000.000000000000000 ) ;
#24814 = EDGE_CURVE ( 'NONE', #17184, #4162, #14899, .T. ) ;
#24815 = CARTESIAN_POINT ( 'NONE',  ( -305.0000000000001137, -152.0000000000000284, 60.00000000000002842 ) ) ;
#24816 = FACE_OUTER_BOUND ( 'NONE', #6920, .T. ) ;
#24817 = PLANE ( 'NONE',  #18880 ) ;
#24818 = ORIENTED_EDGE ( 'NONE', *, *, #27695, .F. ) ;
#24819 = VECTOR ( 'NONE', #15630, 1000.000000000000000 ) ;
#24820 = LINE ( 'NONE', #11900, #12992 ) ;
#24821 = ORIENTED_EDGE ( 'NONE', *, *, #21315, .T. ) ;
#24822 =( LENGTH_UNIT ( ) NAMED_UNIT ( * ) SI_UNIT ( .MILLI., .METRE. ) );
#24823 = EDGE_CURVE ( 'NONE', #17780, #14086, #5976, .T. ) ;
#24824 = ORIENTED_EDGE ( 'NONE', *, *, #4702, .T. ) ;
#24825 = ADVANCED_FACE ( 'NONE', ( #27936 ), #23228, .F. ) ;
#24826 = ORIENTED_EDGE ( 'NONE', *, *, #1064, .T. ) ;
#24827 = EDGE_LOOP ( 'NONE', ( #15931, #27109 ) ) ;
#24828 = ORIENTED_EDGE ( 'NONE', *, *, #13450, .T. ) ;
#24829 = CARTESIAN_POINT ( 'NONE',  ( -156.4100387916780335, 122.2070193974234229, 19.70550239271524973 ) ) ;
#24830 = CARTESIAN_POINT ( 'NONE',  ( 156.9574749595459764, 213.0812361363529988, 45.00000000000000000 ) ) ;
#24831 = CARTESIAN_POINT ( 'NONE',  ( 367.9108539694884144, -5.589247009368149222, 1.243177022048955014E-14 ) ) ;
#24832 = AXIS2_PLACEMENT_3D ( 'NONE', #2033, #23732, #10663 ) ;
#24833 = CARTESIAN_POINT ( 'NONE',  ( -52.57787683962911984, 133.2861237126421088, -15.71127553108205177 ) ) ;
#24834 = EDGE_CURVE ( 'NONE', #1913, #4814, #25796, .T. ) ;
#24835 = CARTESIAN_POINT ( 'NONE',  ( 157.4999999999998579, 55.73418700828869277, 45.00000000000000000 ) ) ;
#24836 = CIRCLE ( 'NONE', #18414, 39.99999999999999289 ) ;
#24837 = CARTESIAN_POINT ( 'NONE',  ( -214.0051257764050945, 55.38571953469081421, 43.60894023861363422 ) ) ;
#24838 = CARTESIAN_POINT ( 'NONE',  ( 157.9999999999998010, 239.0630000600560550, 45.00000000000000000 ) ) ;
#24839 = CARTESIAN_POINT ( 'NONE',  ( -149.4295825701717320, 124.9919708967672989, -17.80889158364129798 ) ) ;
#24840 = DIRECTION ( 'NONE',  ( -1.000000000000000000, 0.000000000000000000, 0.000000000000000000 ) ) ;
#24841 = PLANE ( 'NONE',  #716 ) ;
#24842 = DIRECTION ( 'NONE',  ( 1.000000000000000000, -0.000000000000000000, -0.000000000000000000 ) ) ;
#24843 = CARTESIAN_POINT ( 'NONE',  ( 121.6232796275294277, 239.4748271322486630, 45.00000000000000000 ) ) ;
#24844 = CARTESIAN_POINT ( 'NONE',  ( -210.0000000000000568, -157.0000000000000284, 95.00000000000004263 ) ) ;
#24845 = DIRECTION ( 'NONE',  ( 0.4999999999999985012, -0.8660254037844394848, 0.000000000000000000 ) ) ;
#24846 = CARTESIAN_POINT ( 'NONE',  ( 117.1152841538456926, 116.0550883417529491, -100.0000000000000142 ) ) ;
#24847 = LINE ( 'NONE', #22260, #5179 ) ;
#24849 = ORIENTED_EDGE ( 'NONE', *, *, #5827, .T. ) ;
#24848 = EDGE_LOOP ( 'NONE', ( #5950, #9057, #16405, #18185 ) ) ;
#24850 = DIRECTION ( 'NONE',  ( 1.000000000000000000, 0.000000000000000000, -0.000000000000000000 ) ) ;
#24851 = AXIS2_PLACEMENT_3D ( 'NONE', #26240, #13328, #20205 ) ;
#24852 = LINE ( 'NONE', #17278, #2866 ) ;
#24853 = ORIENTED_EDGE ( 'NONE', *, *, #4629, .F. ) ;
#24854 = VECTOR ( 'NONE', #28218, 1000.000000000000000 ) ;
#24855 = EDGE_LOOP ( 'NONE', ( #24883, #18423, #20854, #27038 ) ) ;
#24856 = AXIS2_PLACEMENT_3D ( 'NONE', #24527, #19783, #17918 ) ;
#24857 = CARTESIAN_POINT ( 'NONE',  ( 157.4999999999998579, 148.5255622860493077, 45.00000000000000000 ) ) ;
#24858 = CARTESIAN_POINT ( 'NONE',  ( -151.8743502727079999, 124.0639289416861288, 18.38162538368994703 ) ) ;
#24859 = ORIENTED_EDGE ( 'NONE', *, *, #28284, .F. ) ;
#24860 = ORIENTED_EDGE ( 'NONE', *, *, #13484, .F. ) ;
#24861 = CARTESIAN_POINT ( 'NONE',  ( -169.4361096980427135, 115.4683091757704005, -26.67336330034965997 ) ) ;
#24862 = CARTESIAN_POINT ( 'NONE',  ( 124.9999999999998579, 220.0000000000000284, -90.00000000000002842 ) ) ;
#24863 = EDGE_CURVE ( 'NONE', #18505, #23832, #12606, .T. ) ;
#24864 = CARTESIAN_POINT ( 'NONE',  ( 47.90501010967909679, 226.8374036014029969, -45.00000000000000000 ) ) ;
#24865 = ADVANCED_FACE ( 'NONE', ( #12324 ), #3531, .F. ) ;
#24866 = LINE ( 'NONE', #20407, #5459 ) ;
#24867 = LINE ( 'NONE', #9783, #26304 ) ;
#24868 = AXIS2_PLACEMENT_3D ( 'NONE', #5650, #8229, #10385 ) ;
#24869 = DIRECTION ( 'NONE',  ( 0.8916010070298252543, -0.4528218681373520904, 0.000000000000000000 ) ) ;
#24870 = VECTOR ( 'NONE', #15997, 1000.000000000000000 ) ;
#24871 = CARTESIAN_POINT ( 'NONE',  ( 3.469446951953618133E-15, -40.00000000000003553, -100.0000000000000142 ) ) ;
#24872 = CARTESIAN_POINT ( 'NONE',  ( -214.1250002713545086, 55.22895589251590565, -44.08339233875913976 ) ) ;
#24873 = FACE_OUTER_BOUND ( 'NONE', #12543, .T. ) ;
#24874 = DIRECTION ( 'NONE',  ( -0.8916010070293384215, 0.4528218681383106015, 0.000000000000000000 ) ) ;
#24875 = FACE_OUTER_BOUND ( 'NONE', #2190, .T. ) ;
#24876 = DIRECTION ( 'NONE',  ( 0.000000000000000000, 0.000000000000000000, 1.000000000000000000 ) ) ;
#24877 = ORIENTED_EDGE ( 'NONE', *, *, #25514, .T. ) ;
#24878 = DIRECTION ( 'NONE',  ( 0.8916010070296936929, -0.4528218681376112165, 0.000000000000000000 ) ) ;
#24879 = EDGE_CURVE ( 'NONE', #4884, #13125, #6123, .T. ) ;
#24880 = CARTESIAN_POINT ( 'NONE',  ( -242.5499235585427584, 73.68467268308823748, 14.74213902348265393 ) ) ;
#24881 = DIRECTION ( 'NONE',  ( 0.000000000000000000, 0.000000000000000000, -1.000000000000000000 ) ) ;
#24882 = VERTEX_POINT ( 'NONE', #1801 ) ;
#24883 = ORIENTED_EDGE ( 'NONE', *, *, #22661, .T. ) ;
#24884 = CIRCLE ( 'NONE', #16187, 5.999999999999977796 ) ;
#24885 = DIRECTION ( 'NONE',  ( 0.000000000000000000, -1.000000000000000000, 0.000000000000000000 ) ) ;
#24886 = PLANE ( 'NONE',  #1638 ) ;
#24887 = ORIENTED_EDGE ( 'NONE', *, *, #2401, .T. ) ;
#24888 = ADVANCED_FACE ( 'NONE', ( #21065 ), #18633, .F. ) ;
#24889 = VECTOR ( 'NONE', #13377, 1000.000000000000000 ) ;
#24890 = EDGE_LOOP ( 'NONE', ( #2093, #19546, #26263, #12752 ) ) ;
#24891 = EDGE_CURVE ( 'NONE', #6895, #19138, #16786, .T. ) ;
#24892 = CARTESIAN_POINT ( 'NONE',  ( -279.3160071107327553, -512.7211954420570237, 0.000000000000000000 ) ) ;
#24893 = VECTOR ( 'NONE', #20534, 1000.000000000000000 ) ;
#24894 = EDGE_CURVE ( 'NONE', #7688, #9244, #6403, .T. ) ;
#24895 = DIRECTION ( 'NONE',  ( -0.8916010070295922185, -0.4528218681378110566, 0.000000000000000000 ) ) ;
#24896 = ADVANCED_FACE ( 'NONE', ( #228 ), #17458, .F. ) ;
#24897 = DIRECTION ( 'NONE',  ( 0.000000000000000000, 0.000000000000000000, -1.000000000000000000 ) ) ;
#24898 = ORIENTED_EDGE ( 'NONE', *, *, #19350, .F. ) ;
#24899 = CARTESIAN_POINT ( 'NONE',  ( 158.0000000000015916, 55.48024950453520177, 45.00000000000000000 ) ) ;
#24900 = ORIENTED_EDGE ( 'NONE', *, *, #3548, .T. ) ;
#24901 = CARTESIAN_POINT ( 'NONE',  ( 157.4999999999998579, 220.0000000000000284, -105.0000000000000284 ) ) ;
#24902 = LINE ( 'NONE', #5070, #25489 ) ;
#24903 = DIRECTION ( 'NONE',  ( -0.000000000000000000, 1.000000000000000000, -1.387778780781445429E-16 ) ) ;
#24904 = CARTESIAN_POINT ( 'NONE',  ( -18.15357532044453137, 129.9610192713841741, -15.33575750053543985 ) ) ;
#24905 = CARTESIAN_POINT ( 'NONE',  ( 158.0000000000009095, 118.6849996997183041, 45.00000000000000000 ) ) ;
#24906 = VECTOR ( 'NONE', #8292, 1000.000000000000000 ) ;
#24907 = LINE ( 'NONE', #27052, #23902 ) ;
#24908 = CARTESIAN_POINT ( 'NONE',  ( 158.0000000000000284, 205.9527499549551806, 45.00000000000000000 ) ) ;
#24909 = VERTEX_POINT ( 'NONE', #11144 ) ;
#24910 = CARTESIAN_POINT ( 'NONE',  ( 133.3333333333334849, -226.6666666666664582, 176.6666666666667425 ) ) ;
#24911 = DIRECTION ( 'NONE',  ( 0.8916010070293384215, 0.4528218681383106015, 0.000000000000000000 ) ) ;
#24913 = DIRECTION ( 'NONE',  ( 0.9506505318133544602, 0.3102637045530566295, 0.000000000000000000 ) ) ;
#24912 = AXIS2_PLACEMENT_3D ( 'NONE', #7836, #12307, #7421 ) ;
#24914 = CARTESIAN_POINT ( 'NONE',  ( 157.9999999999998295, 226.0157500150140208, 45.00000000000000000 ) ) ;
#24915 = ORIENTED_EDGE ( 'NONE', *, *, #17613, .F. ) ;
#24916 = CARTESIAN_POINT ( 'NONE',  ( -146.6428522700808230, 69.54464929955099706, 83.00000000000001421 ) ) ;
#24917 = ORIENTED_EDGE ( 'NONE', *, *, #15070, .T. ) ;
#24918 = DIRECTION ( 'NONE',  ( -0.000000000000000000, -0.000000000000000000, -1.000000000000000000 ) ) ;
#24919 = DIRECTION ( 'NONE',  ( 1.000000000000000000, -0.000000000000000000, -0.000000000000000000 ) ) ;
#24920 = ORIENTED_EDGE ( 'NONE', *, *, #20668, .F. ) ;
#24921 = DIRECTION ( 'NONE',  ( 0.4528218681370511089, -0.8916010070299782431, 0.000000000000000000 ) ) ;
#24922 = CARTESIAN_POINT ( 'NONE',  ( -112.3221550338875687, 69.54464929955099706, 83.00000000000001421 ) ) ;
#24923 = ORIENTED_EDGE ( 'NONE', *, *, #587, .T. ) ;
#24924 = EDGE_CURVE ( 'NONE', #8056, #2800, #5761, .T. ) ;
#24925 = ADVANCED_FACE ( 'NONE', ( #17742 ), #82, .T. ) ;
#24926 = FACE_OUTER_BOUND ( 'NONE', #12816, .T. ) ;
#24927 = CARTESIAN_POINT ( 'NONE',  ( 89.99999999999988631, 240.0000000000000284, 6.270166537925822681 ) ) ;
#24928 = ORIENTED_EDGE ( 'NONE', *, *, #21052, .T. ) ;
#24929 = VECTOR ( 'NONE', #2917, 1000.000000000000000 ) ;
#24930 = VERTEX_POINT ( 'NONE', #1941 ) ;
#24931 = EDGE_CURVE ( 'NONE', #27204, #3702, #26130, .T. ) ;
#24932 = DIRECTION ( 'NONE',  ( 1.000000000000000000, 1.321694076934710155E-16, -0.000000000000000000 ) ) ;
#24933 = VERTEX_POINT ( 'NONE', #17315 ) ;
#24934 = AXIS2_PLACEMENT_3D ( 'NONE', #12703, #3773, #12562 ) ;
#24935 = EDGE_CURVE ( 'NONE', #5617, #10903, #2830, .T. ) ;
#24936 = VERTEX_POINT ( 'NONE', #10577 ) ;
#24937 = VERTEX_POINT ( 'NONE', #6545 ) ;
#24938 = VECTOR ( 'NONE', #28379, 1000.000000000000000 ) ;
#24939 = CARTESIAN_POINT ( 'NONE',  ( 179.9999999999999147, -5.589247009368157215, 84.99999999999997158 ) ) ;
#24940 = CARTESIAN_POINT ( 'NONE',  ( -73.64246817076464424, 87.16319020291010133, -145.0000000000000000 ) ) ;
#24941 = DIRECTION ( 'NONE',  ( 0.000000000000000000, -9.486769009248163798E-17, 1.000000000000000000 ) ) ;
#24942 = DIRECTION ( 'NONE',  ( 0.8916010070299273949, 0.4528218681371510290, 0.000000000000000000 ) ) ;
#24943 = DIRECTION ( 'NONE',  ( -0.7071067811865336949, 0.7071067811865613395, 0.000000000000000000 ) ) ;
#24944 = DIRECTION ( 'NONE',  ( 1.000000000000000000, 0.000000000000000000, 0.000000000000000000 ) ) ;
#24945 = CARTESIAN_POINT ( 'NONE',  ( 158.0000000000002842, 180.8739998798873501, 45.00000000000000000 ) ) ;
#24946 = DIRECTION ( 'NONE',  ( 1.530283246943720875E-16, -1.000000000000000000, 0.000000000000000000 ) ) ;
#24947 = CARTESIAN_POINT ( 'NONE',  ( -190.0000000000000284, -40.00000000000004974, 98.28427124746191623 ) ) ;
#24948 = CARTESIAN_POINT ( 'NONE',  ( 158.0000000000011084, 100.6219996396619791, 45.00000000000000000 ) ) ;
#24949 = DIRECTION ( 'NONE',  ( 0.000000000000000000, 1.000000000000000000, 0.000000000000000000 ) ) ;
#24950 = VERTEX_POINT ( 'NONE', #4243 ) ;
#24951 = VECTOR ( 'NONE', #8180, 1000.000000000000000 ) ;
#24952 = VECTOR ( 'NONE', #7070, 1000.000000000000227 ) ;
#24953 = CARTESIAN_POINT ( 'NONE',  ( -277.2150368962633706, -165.0000000000001421, 90.47363622314040299 ) ) ;
#24954 = CARTESIAN_POINT ( 'NONE',  ( 114.5814157129578916, 209.3660254037841923, -45.00000000000000000 ) ) ;
#24955 = CARTESIAN_POINT ( 'NONE',  ( -143.6428522700808230, 20.24192588826928585, 93.88690167569083656 ) ) ;
#24956 = AXIS2_PLACEMENT_3D ( 'NONE', #16338, #27646, #7708 ) ;
#24957 = ORIENTED_EDGE ( 'NONE', *, *, #12521, .T. ) ;
#24958 = EDGE_CURVE ( 'NONE', #1444, #1356, #19333, .T. ) ;
#24959 = CARTESIAN_POINT ( 'NONE',  ( 134.9999999999998579, 268.4896896257338881, 84.99999999999995737 ) ) ;
#24960 = ORIENTED_EDGE ( 'NONE', *, *, #205, .T. ) ;
#24961 = LINE ( 'NONE', #22809, #1740 ) ;
#24962 = EDGE_LOOP ( 'NONE', ( #21176, #15431 ) ) ;
#24963 = ORIENTED_EDGE ( 'NONE', *, *, #1149, .T. ) ;
#24964 = ORIENTED_EDGE ( 'NONE', *, *, #3904, .F. ) ;
#24965 = B_SPLINE_CURVE_WITH_KNOTS ( 'NONE', 3,
 ( #7522, #16423, #11407, #4394, #15866, #1601, #1321, #14835, #12261, #8073, #3607, #3748, #3896, #28017, #5772, #14546, #12402, #8214, #10092, #23302, #14268, #21138 ),
 .UNSPECIFIED., .F., .F.,
 ( 4, 2, 2, 2, 2, 2, 2, 2, 2, 2, 4 ),
 ( 0.000000000000000000, 0.06249999999999987510, 0.1249999999999999306, 0.1875000000000000000, 0.2500000000000000555, 0.3750000000000000000, 0.5000000000000000000, 0.6250000000000000000, 0.7500000000000000000, 0.8750000000000001110, 1.000000000000000000 ),
 .UNSPECIFIED. ) ;
#24966 = ORIENTED_EDGE ( 'NONE', *, *, #16608, .T. ) ;
#24967 = CARTESIAN_POINT ( 'NONE',  ( -77.61721128200930764, 136.2551396520290723, 13.51936372730774849 ) ) ;
#24968 = AXIS2_PLACEMENT_3D ( 'NONE', #4075, #10837, #12861 ) ;
#24969 = CARTESIAN_POINT ( 'NONE',  ( 179.9999999999999147, 0.000000000000000000, 84.99999999999995737 ) ) ;
#24970 = FACE_OUTER_BOUND ( 'NONE', #26560, .T. ) ;
#24971 = EDGE_CURVE ( 'NONE', #15116, #3105, #22056, .T. ) ;
#24972 = DIRECTION ( 'NONE',  ( 0.000000000000000000, 0.000000000000000000, -1.000000000000000000 ) ) ;
#24973 = EDGE_CURVE ( 'NONE', #13125, #15105, #15467, .T. ) ;
#24974 = VECTOR ( 'NONE', #19573, 1000.000000000000000 ) ;
#24975 = CARTESIAN_POINT ( 'NONE',  ( -23.64013312899696828, 129.3207233730292955, 15.61661841831484132 ) ) ;
#24976 = CARTESIAN_POINT ( 'NONE',  ( -207.5108889574473494, 75.59417117316073131, 44.26576816510100798 ) ) ;
#24977 = CARTESIAN_POINT ( 'NONE',  ( 158.0000000000013358, 80.55899957960563995, 45.00000000000000000 ) ) ;
#24978 = CARTESIAN_POINT ( 'NONE',  ( -47.47907723713406369, 132.2277457862344932, -14.48493892500291835 ) ) ;
#24979 = CARTESIAN_POINT ( 'NONE',  ( 79.99999999999995737, 87.77847705527369726, -99.04049946057673992 ) ) ;
#24980 = CARTESIAN_POINT ( 'NONE',  ( 232.4999999999996305, 133.0668745871126930, 42.86484227207692044 ) ) ;
#24981 = CARTESIAN_POINT ( 'NONE',  ( 157.4999999999998579, 90.84443711338730054, 45.00000000000000000 ) ) ;
#24982 = CARTESIAN_POINT ( 'NONE',  ( 217.4999999999996305, 194.4107529906318064, -100.0000000000000000 ) ) ;
#24983 = ADVANCED_FACE ( 'NONE', ( #21915 ), #8703, .F. ) ;
#24984 = ADVANCED_FACE ( 'NONE', ( #2220 ), #8427, .T. ) ;
#24985 = PLANE ( 'NONE',  #24755 ) ;
#24986 = CARTESIAN_POINT ( 'NONE',  ( -188.7721129603572194, 104.0449037398145009, 32.78712893570086351 ) ) ;
#24987 = DIRECTION ( 'NONE',  ( -0.000000000000000000, -0.000000000000000000, -1.000000000000000000 ) ) ;
#24989 = VERTEX_POINT ( 'NONE', #15326 ) ;
#24988 = ORIENTED_EDGE ( 'NONE', *, *, #11907, .T. ) ;
#24990 = AXIS2_PLACEMENT_3D ( 'NONE', #10520, #4038, #14554 ) ;
#24991 = EDGE_CURVE ( 'NONE', #9161, #12189, #15034, .T. ) ;
#24992 = DIRECTION ( 'NONE',  ( 1.000000000000000000, -0.000000000000000000, 0.000000000000000000 ) ) ;
#24993 = EDGE_LOOP ( 'NONE', ( #27571, #22727 ) ) ;
#24994 = AXIS2_PLACEMENT_3D ( 'NONE', #7434, #2682, #9303 ) ;
#24995 = ORIENTED_EDGE ( 'NONE', *, *, #16083, .F. ) ;
#24996 = DIRECTION ( 'NONE',  ( -0.8379557447115515423, 0.5457381880580733924, 0.000000000000000000 ) ) ;
#24997 = CARTESIAN_POINT ( 'NONE',  ( -77.72059375409217807, 134.6165094220598917, 15.48686464813458841 ) ) ;
#24998 = ORIENTED_EDGE ( 'NONE', *, *, #3738, .T. ) ;
#24999 = ORIENTED_EDGE ( 'NONE', *, *, #4629, .T. ) ;
#25000 = CARTESIAN_POINT ( 'NONE',  ( 158.0000000000010800, 101.1298746471690038, 45.00000000000000000 ) ) ;
#25001 = FACE_OUTER_BOUND ( 'NONE', #19118, .T. ) ;
#25002 = EDGE_CURVE ( 'NONE', #23711, #20791, #18184, .T. ) ;
#25003 = EDGE_CURVE ( 'NONE', #14031, #3490, #11730, .T. ) ;
#25004 = DIRECTION ( 'NONE',  ( -1.000000000000000000, -0.000000000000000000, -0.000000000000000000 ) ) ;
#25005 = VECTOR ( 'NONE', #18198, 1000.000000000000000 ) ;
#25006 = TOROIDAL_SURFACE ( 'NONE', #17676, 44.99999999999999289, 5.000000000000000000 ) ;
#25007 = VECTOR ( 'NONE', #24869, 1000.000000000000114 ) ;
#25008 = CARTESIAN_POINT ( 'NONE',  ( -66.26041567618258910, 130.4659900502583127, -45.00000000000000000 ) ) ;
#25009 = CARTESIAN_POINT ( 'NONE',  ( 157.4999999999998010, 238.8090625563025071, 45.00000000000000000 ) ) ;
#25010 = AXIS2_PLACEMENT_3D ( 'NONE', #2043, #25894, #17276 ) ;
#25011 = CARTESIAN_POINT ( 'NONE',  ( 134.9999999999998579, 220.0000000000000284, -99.00000000000001421 ) ) ;
#25012 = CARTESIAN_POINT ( 'NONE',  ( -213.4823095283139196, 56.20074567116226660, -41.47858424781075115 ) ) ;
#25013 = EDGE_CURVE ( 'NONE', #23789, #4844, #11295, .T. ) ;
#25014 = PLANE ( 'NONE',  #24250 ) ;
#25015 = CARTESIAN_POINT ( 'NONE',  ( 157.4999999999998579, 223.7618125112605298, 45.00000000000000000 ) ) ;
#25016 = LINE ( 'NONE', #9653, #13427 ) ;
#25017 = PLANE ( 'NONE',  #9374 ) ;
#25018 = ORIENTED_EDGE ( 'NONE', *, *, #19877, .T. ) ;
#25019 = ADVANCED_FACE ( 'NONE', ( #13887 ), #11592, .F. ) ;
#25020 = CARTESIAN_POINT ( 'NONE',  ( -231.9378824387731299, 93.53122965655668963, -13.00000000000000000 ) ) ;
#25021 = EDGE_CURVE ( 'NONE', #13173, #6225, #7148, .T. ) ;
#25022 = CARTESIAN_POINT ( 'NONE',  ( -230.6867234551439196, 75.40543009380269268, 15.98884730490149764 ) ) ;
#25023 = CARTESIAN_POINT ( 'NONE',  ( -68.57415822541635464, -23.01420295945612082, 95.00000000000000000 ) ) ;
#25024 = ORIENTED_EDGE ( 'NONE', *, *, #6300, .F. ) ;
#25025 = DIRECTION ( 'NONE',  ( 1.000000000000000000, 0.000000000000000000, 0.000000000000000000 ) ) ;
#25026 = AXIS2_PLACEMENT_3D ( 'NONE', #13860, #22748, #9538 ) ;
#25027 = ADVANCED_FACE ( 'NONE', ( #7407 ), #15752, .F. ) ;
#25028 = EDGE_LOOP ( 'NONE', ( #5085, #6362, #17399, #2189 ) ) ;
#25029 = AXIS2_PLACEMENT_3D ( 'NONE', #24370, #28376, #17200 ) ;
#25030 = LINE ( 'NONE', #20431, #6033 ) ;
#25031 = PLANE ( 'NONE',  #19547 ) ;
#25032 = ORIENTED_EDGE ( 'NONE', *, *, #10620, .F. ) ;
#25033 = AXIS2_PLACEMENT_3D ( 'NONE', #14115, #20846, #9934 ) ;
#25034 = ORIENTED_EDGE ( 'NONE', *, *, #20216, .F. ) ;
#25035 = LINE ( 'NONE', #16138, #23261 ) ;
#25036 = CYLINDRICAL_SURFACE ( 'NONE', #10201, 64.76834224489934400 ) ;
#25037 = DIRECTION ( 'NONE',  ( -0.000000000000000000, -0.000000000000000000, -1.000000000000000000 ) ) ;
#25039 = ADVANCED_FACE ( 'NONE', ( #13593 ), #26938, .F. ) ;
#25038 = ORIENTED_EDGE ( 'NONE', *, *, #13201, .T. ) ;
#25040 = CARTESIAN_POINT ( 'NONE',  ( 141.9187638636471434, 198.0425250404537678, -45.00000000000000000 ) ) ;
#25041 = ORIENTED_EDGE ( 'NONE', *, *, #674, .T. ) ;
#25042 = DIRECTION ( 'NONE',  ( 1.000000000000000000, 0.000000000000000000, 0.000000000000000000 ) ) ;
#25043 = DIRECTION ( 'NONE',  ( -0.8660254037844362651, 0.5000000000000039968, -0.000000000000000000 ) ) ;
#25044 = VECTOR ( 'NONE', #25175, 1000.000000000000000 ) ;
#25045 = CARTESIAN_POINT ( 'NONE',  ( 109.9999999999999147, 140.0000000000000000, -90.00000000000004263 ) ) ;
#25046 = CARTESIAN_POINT ( 'NONE',  ( 6.408192432492758606, 140.2484972092699138, -14.93046625219126078 ) ) ;
#25047 = VECTOR ( 'NONE', #5110, 1000.000000000000000 ) ;
#25048 = LINE ( 'NONE', #13863, #2221 ) ;
#25049 = DIRECTION ( 'NONE',  ( 0.8314772792026879911, -0.5555587585212703461, 0.000000000000000000 ) ) ;
#25050 = PLANE ( 'NONE',  #8110 ) ;
#25051 = ORIENTED_EDGE ( 'NONE', *, *, #22756, .T. ) ;
#25052 = CARTESIAN_POINT ( 'NONE',  ( 157.4999999999998579, 60.74993702330277756, 45.00000000000000000 ) ) ;
#25053 = CIRCLE ( 'NONE', #13604, 5.000000000000004441 ) ;
#25054 = CARTESIAN_POINT ( 'NONE',  ( 157.9999999999997726, 248.5866250825770294, 45.00000000000000000 ) ) ;
#25055 = CARTESIAN_POINT ( 'NONE',  ( 157.4999999999997442, 256.3641876088515232, 45.00000000000000000 ) ) ;
#25056 = ORIENTED_EDGE ( 'NONE', *, *, #6019, .T. ) ;
#25057 = EDGE_CURVE ( 'NONE', #12396, #24423, #17531, .T. ) ;
#25058 = DIRECTION ( 'NONE',  ( -0.2066290158914688424, -0.9784193629480781862, 0.000000000000000000 ) ) ;
#25059 = EDGE_CURVE ( 'NONE', #4836, #8677, #24789, .T. ) ;
#25060 = ORIENTED_EDGE ( 'NONE', *, *, #240, .T. ) ;
#25061 = CARTESIAN_POINT ( 'NONE',  ( -217.2892621185082760, 109.4029876883478352, -13.00000000000000000 ) ) ;
#25062 = CARTESIAN_POINT ( 'NONE',  ( 199.9999999999998863, -280.0000000000000000, 110.0000000000000284 ) ) ;
#25063 = DIRECTION ( 'NONE',  ( 0.000000000000000000, 0.7071067811865455743, -0.7071067811865493491 ) ) ;
#25064 = ORIENTED_EDGE ( 'NONE', *, *, #17321, .F. ) ;
#25065 = CARTESIAN_POINT ( 'NONE',  ( 0.000000000000000000, 0.000000000000000000, 0.000000000000000000 ) ) ;
#25066 = DIRECTION ( 'NONE',  ( 1.000000000000000000, 0.000000000000000000, 0.000000000000000000 ) ) ;
#25067 = ORIENTED_EDGE ( 'NONE', *, *, #25462, .T. ) ;
#25068 = CARTESIAN_POINT ( 'NONE',  ( -67.66005108804499457, 133.9293368352053051, 15.61826086920359913 ) ) ;
#25069 = CARTESIAN_POINT ( 'NONE',  ( 105.0441603316952381, 246.7663426280820147, 21.68296015126954401 ) ) ;
#25070 = VERTEX_POINT ( 'NONE', #7263 ) ;
#25071 = AXIS2_PLACEMENT_3D ( 'NONE', #19621, #86, #15184 ) ;
#25072 = ORIENTED_EDGE ( 'NONE', *, *, #13852, .T. ) ;
#25073 = CARTESIAN_POINT ( 'NONE',  ( -210.0000000000000568, -157.0000000000000284, -94.99999999999987210 ) ) ;
#25074 = ORIENTED_EDGE ( 'NONE', *, *, #2331, .F. ) ;
#25075 = ORIENTED_EDGE ( 'NONE', *, *, #6294, .T. ) ;
#25076 = AXIS2_PLACEMENT_3D ( 'NONE', #11886, #20347, #2814 ) ;
#25077 = VERTEX_POINT ( 'NONE', #2945 ) ;
#25078 = DIRECTION ( 'NONE',  ( -0.000000000000000000, -0.000000000000000000, -1.000000000000000000 ) ) ;
#25079 = DIRECTION ( 'NONE',  ( -0.8660254037844362651, 0.5000000000000039968, -0.000000000000000000 ) ) ;
#25080 = LINE ( 'NONE', #3087, #27515 ) ;
#25081 = CARTESIAN_POINT ( 'NONE',  ( 158.0000000000005400, 155.7952498048169048, 45.00000000000000000 ) ) ;
#25082 = LINE ( 'NONE', #11883, #16326 ) ;
#25083 = DIRECTION ( 'NONE',  ( 1.000000000000000000, 0.000000000000000000, -0.000000000000000000 ) ) ;
#25084 = DIRECTION ( 'NONE',  ( 0.7348549764921636918, -0.6782242722910333255, 0.000000000000000000 ) ) ;
#25085 = DIRECTION ( 'NONE',  ( 0.000000000000000000, 0.000000000000000000, -1.000000000000000000 ) ) ;
#25086 = CARTESIAN_POINT ( 'NONE',  ( 206.2214737538543829, 104.7347325308398354, 45.00000000000000000 ) ) ;
#25087 = PLANE ( 'NONE',  #28129 ) ;
#25088 = AXIS2_PLACEMENT_3D ( 'NONE', #24792, #27078, #5247 ) ;
#25089 = ORIENTED_EDGE ( 'NONE', *, *, #26538, .F. ) ;
#25090 = EDGE_CURVE ( 'NONE', #23123, #7575, #20329, .T. ) ;
#25091 = EDGE_CURVE ( 'NONE', #7226, #5857, #4862, .T. ) ;
#25092 = LINE ( 'NONE', #25508, #20627 ) ;
#25093 = CYLINDRICAL_SURFACE ( 'NONE', #14000, 5.000000000000004441 ) ;
#25094 = DIRECTION ( 'NONE',  ( 0.8660254037844455910, 0.4999999999999881206, 0.000000000000000000 ) ) ;
#25095 = ORIENTED_EDGE ( 'NONE', *, *, #27281, .F. ) ;
#25096 = DIRECTION ( 'NONE',  ( -1.000000000000000000, 0.000000000000000000, 0.000000000000000000 ) ) ;
#25097 = ORIENTED_EDGE ( 'NONE', *, *, #21846, .T. ) ;
#25098 = DIRECTION ( 'NONE',  ( 0.8916010070295922185, -0.4528218681378110566, 0.000000000000000000 ) ) ;
#25099 = ORIENTED_EDGE ( 'NONE', *, *, #14307, .F. ) ;
#25100 = ORIENTED_EDGE ( 'NONE', *, *, #18802, .F. ) ;
#25101 = ORIENTED_EDGE ( 'NONE', *, *, #18993, .T. ) ;
#25102 = EDGE_LOOP ( 'NONE', ( #1250, #20982, #27452, #9315 ) ) ;
#25103 = CARTESIAN_POINT ( 'NONE',  ( -144.8714485210765304, 126.6523762207952757, 16.84425668626998984 ) ) ;
#25104 = VECTOR ( 'NONE', #6049, 1000.000000000000114 ) ;
#25105 = DIRECTION ( 'NONE',  ( -0.000000000000000000, -0.000000000000000000, 1.000000000000000000 ) ) ;
#25106 = CARTESIAN_POINT ( 'NONE',  ( 158.0000000000015348, 58.49599951954928656, 45.00000000000000000 ) ) ;
#25107 = DIRECTION ( 'NONE',  ( 0.000000000000000000, 0.000000000000000000, -1.000000000000000000 ) ) ;
#25108 = CARTESIAN_POINT ( 'NONE',  ( -194.2478650485211062, 63.21120109188145619, 44.02102422013626892 ) ) ;
#25109 = CARTESIAN_POINT ( 'NONE',  ( 157.9999999999998010, 234.0472500450420341, -45.00000000000000000 ) ) ;
#25110 = EDGE_CURVE ( 'NONE', #4442, #1347, #7687, .T. ) ;
#25111 = CARTESIAN_POINT ( 'NONE',  ( 134.9999999999998579, 457.0747856552986832, -137.4901433416540328 ) ) ;
#25112 = FACE_OUTER_BOUND ( 'NONE', #11769, .T. ) ;
#25113 = CARTESIAN_POINT ( 'NONE',  ( 157.4999999999998579, 85.82868709837320864, 45.00000000000000000 ) ) ;
#25114 = PRESENTATION_STYLE_ASSIGNMENT (( #1125 ) ) ;
#25115 = DIRECTION ( 'NONE',  ( -0.4528218681382754629, 0.8916010070293562961, 0.000000000000000000 ) ) ;
#25116 = DIRECTION ( 'NONE',  ( -0.9506505318133482429, 0.3102637045530752813, 0.000000000000000000 ) ) ;
#25117 = ORIENTED_EDGE ( 'NONE', *, *, #20047, .T. ) ;
#25118 = EDGE_CURVE ( 'NONE', #26005, #23503, #3501, .T. ) ;
#25119 = LINE ( 'NONE', #9338, #20152 ) ;
#25120 = DIRECTION ( 'NONE',  ( 0.000000000000000000, 0.000000000000000000, -1.000000000000000000 ) ) ;
#25121 = DIRECTION ( 'NONE',  ( -0.8916010070294098089, -0.4528218681381701027, 0.000000000000000000 ) ) ;
#25123 = VERTEX_POINT ( 'NONE', #1212 ) ;
#25122 = ORIENTED_EDGE ( 'NONE', *, *, #21887, .F. ) ;
#25124 = VECTOR ( 'NONE', #23403, 1000.000000000000114 ) ;
#25125 = ADVANCED_FACE ( 'NONE', ( #27625 ), #25201, .F. ) ;
#25126 = CARTESIAN_POINT ( 'NONE',  ( 158.0000000000007390, 135.7322497447605656, 45.00000000000000000 ) ) ;
#25127 = ORIENTED_EDGE ( 'NONE', *, *, #13321, .T. ) ;
#25128 = ORIENTED_EDGE ( 'NONE', *, *, #18923, .F. ) ;
#25129 = ORIENTED_EDGE ( 'NONE', *, *, #13849, .T. ) ;
#25130 = ORIENTED_EDGE ( 'NONE', *, *, #27716, .T. ) ;
#25131 = ORIENTED_EDGE ( 'NONE', *, *, #17487, .F. ) ;
#25132 = LINE ( 'NONE', #22986, #11060 ) ;
#25133 = EDGE_CURVE ( 'NONE', #11334, #4392, #27484, .T. ) ;
#25134 = CYLINDRICAL_SURFACE ( 'NONE', #3540, 5.999999999999991118 ) ;
#25135 = AXIS2_PLACEMENT_3D ( 'NONE', #10316, #22967, #1552 ) ;
#25136 = VECTOR ( 'NONE', #7390, 1000.000000000000000 ) ;
#25137 = CARTESIAN_POINT ( 'NONE',  ( 157.9999999999996305, 281.6968751876750616, 45.00000000000000000 ) ) ;
#25138 = DIRECTION ( 'NONE',  ( 0.000000000000000000, -1.000000000000000000, 0.000000000000000000 ) ) ;
#25139 = CYLINDRICAL_SURFACE ( 'NONE', #23868, 29.99999999999997158 ) ;
#25140 = ADVANCED_FACE ( 'NONE', ( #3783 ), #16451, .F. ) ;
#25141 = DIRECTION ( 'NONE',  ( 0.000000000000000000, -1.000000000000000000, -1.214306433183764966E-16 ) ) ;
#25142 = PLANE ( 'NONE',  #1325 ) ;
#25143 = DIRECTION ( 'NONE',  ( 1.000000000000000000, 0.000000000000000000, 0.000000000000000000 ) ) ;
#25145 = CARTESIAN_POINT ( 'NONE',  ( 111.2314996473659647, 201.6932835404816160, -149.5158039499305573 ) ) ;
#25144 = AXIS2_PLACEMENT_3D ( 'NONE', #19515, #8599, #2829 ) ;
#25146 = DIRECTION ( 'NONE',  ( -0.8660254037844363761, 0.5000000000000041078, -0.000000000000000000 ) ) ;
#25147 = PLANE ( 'NONE',  #27614 ) ;
#25148 = CARTESIAN_POINT ( 'NONE',  ( 0.000000000000000000, 9.154318122686608561E-16, 7.475068018844455153 ) ) ;
#25149 = ORIENTED_EDGE ( 'NONE', *, *, #27114, .T. ) ;
#25150 = CARTESIAN_POINT ( 'NONE',  ( -192.3374199748951412, 101.4858760524708430, 32.80924214881481760 ) ) ;
#25151 = CONICAL_SURFACE ( 'NONE', #394, 6.000000000000005329, 1.029744258676651647 ) ;
#25152 = ADVANCED_FACE ( 'NONE', ( #10400 ), #25614, .F. ) ;
#25153 = ADVANCED_FACE ( 'NONE', ( #12151 ), #25757, .T. ) ;
#25154 = CARTESIAN_POINT ( 'NONE',  ( -237.6054256748464013, 69.18099216265957807, 14.87827728787644155 ) ) ;
#25155 = VECTOR ( 'NONE', #3834, 1000.000000000000000 ) ;
#25156 = CARTESIAN_POINT ( 'NONE',  ( -260.0000000000001137, -167.0819201924624622, 95.00000000000002842 ) ) ;
#25157 = VERTEX_POINT ( 'NONE', #19156 ) ;
#25158 = ORIENTED_EDGE ( 'NONE', *, *, #21099, .T. ) ;
#25159 = DIRECTION ( 'NONE',  ( -0.000000000000000000, -0.000000000000000000, -1.000000000000000000 ) ) ;
#25160 = DIRECTION ( 'NONE',  ( -0.000000000000000000, -0.000000000000000000, -1.000000000000000000 ) ) ;
#25161 = VERTEX_POINT ( 'NONE', #27899 ) ;
#25163 = EDGE_CURVE ( 'NONE', #20475, #21163, #5665, .T. ) ;
#25162 = ORIENTED_EDGE ( 'NONE', *, *, #1571, .F. ) ;
#25164 = DIRECTION ( 'NONE',  ( 1.000000000000000000, 0.000000000000000000, 0.000000000000000000 ) ) ;
#25165 = EDGE_CURVE ( 'NONE', #2951, #22270, #23330, .T. ) ;
#25166 = DIRECTION ( 'NONE',  ( -0.000000000000000000, 0.000000000000000000, 1.000000000000000000 ) ) ;
#25167 = CIRCLE ( 'NONE', #12795, 30.00000000000000000 ) ;
#25168 = CARTESIAN_POINT ( 'NONE',  ( 111.9999999999968878, -1.554312234475174324E-12, 45.00000000000000000 ) ) ;
#25169 = ORIENTED_EDGE ( 'NONE', *, *, #18406, .F. ) ;
#25170 = FACE_OUTER_BOUND ( 'NONE', #15363, .T. ) ;
#25171 = VERTEX_POINT ( 'NONE', #3643 ) ;
#25172 = CARTESIAN_POINT ( 'NONE',  ( 157.4999999999998579, 63.25781203080982351, 45.00000000000000000 ) ) ;
#25173 = AXIS2_PLACEMENT_3D ( 'NONE', #2488, #644, #18022 ) ;
#25174 = VECTOR ( 'NONE', #14102, 1000.000000000000000 ) ;
#25175 = DIRECTION ( 'NONE',  ( -0.000000000000000000, -0.000000000000000000, -1.000000000000000000 ) ) ;
#25176 = EDGE_CURVE ( 'NONE', #13244, #6317, #21169, .T. ) ;
#25177 = CARTESIAN_POINT ( 'NONE',  ( 157.4999999999998579, 68.27356204582390831, 45.00000000000000000 ) ) ;
#25178 = CARTESIAN_POINT ( 'NONE',  ( -42.53273978471831640, 130.9733465240572627, -14.93735646117641025 ) ) ;
#25179 = DIRECTION ( 'NONE',  ( -0.8916010070293584056, 0.4528218681382713551, 0.000000000000000000 ) ) ;
#25180 = CIRCLE ( 'NONE', #2248, 41.00000000000000711 ) ;
#25181 = CARTESIAN_POINT ( 'NONE',  ( 113.0425250404538673, 226.9187638636466602, -45.00000000000000000 ) ) ;
#25182 = CARTESIAN_POINT ( 'NONE',  ( 158.0000000000007674, 133.2243747372535267, 45.00000000000000000 ) ) ;
#25183 = ORIENTED_EDGE ( 'NONE', *, *, #23421, .F. ) ;
#25184 = CARTESIAN_POINT ( 'NONE',  ( 157.4999999999998579, 93.35231212089433939, -45.00000000000000000 ) ) ;
#25185 = CARTESIAN_POINT ( 'NONE',  ( -228.3260857049913000, 133.0445111367240827, 15.00000000000000000 ) ) ;
#25186 = LINE ( 'NONE', #14424, #2011 ) ;
#25187 = ORIENTED_EDGE ( 'NONE', *, *, #18218, .T. ) ;
#25188 = CARTESIAN_POINT ( 'NONE',  ( 158.0000000000014495, 66.01962454207041731, 45.00000000000000000 ) ) ;
#25189 = ORIENTED_EDGE ( 'NONE', *, *, #5032, .F. ) ;
#25190 = VECTOR ( 'NONE', #24068, 1000.000000000000000 ) ;
#25191 = LINE ( 'NONE', #14291, #615 ) ;
#25192 = CARTESIAN_POINT ( 'NONE',  ( -210.0000000000000568, -220.0000000000000853, 109.1217062362809145 ) ) ;
#25193 = LINE ( 'NONE', #20604, #15386 ) ;
#25194 = VERTEX_POINT ( 'NONE', #9840 ) ;
#25195 = FACE_OUTER_BOUND ( 'NONE', #5754, .T. ) ;
#25196 = VECTOR ( 'NONE', #3187, 1000.000000000000000 ) ;
#25197 = DIRECTION ( 'NONE',  ( -0.000000000000000000, 0.000000000000000000, 1.000000000000000000 ) ) ;
#25198 = EDGE_LOOP ( 'NONE', ( #24429, #16977, #19143, #13592, #16459, #24285 ) ) ;
#25199 = VECTOR ( 'NONE', #24845, 1000.000000000000114 ) ;
#25200 = CARTESIAN_POINT ( 'NONE',  ( -133.3218633279795995, 128.8707778179846741, 17.13879255355997699 ) ) ;
#25201 = PLANE ( 'NONE',  #2555 ) ;
#25202 = ORIENTED_EDGE ( 'NONE', *, *, #11814, .F. ) ;
#25203 = ORIENTED_EDGE ( 'NONE', *, *, #16737, .F. ) ;
#25204 = VECTOR ( 'NONE', #9504, 1000.000000000000114 ) ;
#25205 = CARTESIAN_POINT ( 'NONE',  ( -225.7036482868739427, -91.18033988749901653, 0.000000000000000000 ) ) ;
#25206 = ORIENTED_EDGE ( 'NONE', *, *, #9014, .F. ) ;
#25207 = EDGE_LOOP ( 'NONE', ( #1985, #8596, #1521, #24066 ) ) ;
#25208 = ORIENTED_EDGE ( 'NONE', *, *, #23533, .F. ) ;
#25209 = EDGE_CURVE ( 'NONE', #23933, #18077, #14718, .T. ) ;
#25210 = PLANE ( 'NONE',  #9762 ) ;
#25211 = ADVANCED_FACE ( 'NONE', ( #22911 ), #11200, .T. ) ;
#25212 = VECTOR ( 'NONE', #28283, 1000.000000000000000 ) ;
#25213 = CARTESIAN_POINT ( 'NONE',  ( 1.982541115402066017E-14, -150.0000000000000568, 100.0000000000000142 ) ) ;
#25214 = MECHANICAL_DESIGN_GEOMETRIC_PRESENTATION_REPRESENTATION (  '', ( #17353 ), #7280 ) ;
#25215 = DIRECTION ( 'NONE',  ( 1.000000000000000000, 0.000000000000000000, 0.000000000000000000 ) ) ;
#25216 = CARTESIAN_POINT ( 'NONE',  ( 158.0000000000016485, 50.46449948952111697, 45.00000000000000000 ) ) ;
#25217 = AXIS2_PLACEMENT_3D ( 'NONE', #17734, #15597, #20030 ) ;
#25218 = CARTESIAN_POINT ( 'NONE',  ( -63.57415822541634043, -18.01420295945611727, 100.0000000000000000 ) ) ;
#25219 = DIRECTION ( 'NONE',  ( -1.000000000000000000, 0.000000000000000000, 0.000000000000000000 ) ) ;
#25220 = DIRECTION ( 'NONE',  ( -0.8498245983675984938, -0.3891357156574838383, -0.3554877590144110422 ) ) ;
#25221 = CYLINDRICAL_SURFACE ( 'NONE', #18425, 7.499999999999992895 ) ;
#25222 = LINE ( 'NONE', #14048, #3123 ) ;
#25223 = CARTESIAN_POINT ( 'NONE',  ( 113.6021183481336294, 213.0266806119306580, -97.68838206577098049 ) ) ;
#25224 = VERTEX_POINT ( 'NONE', #2613 ) ;
#25225 = VECTOR ( 'NONE', #9608, 1000.000000000000000 ) ;
#25226 = CARTESIAN_POINT ( 'NONE',  ( -7.377946765535823737, 132.9103126869670461, 14.28005041300768951 ) ) ;
#25227 = CARTESIAN_POINT ( 'NONE',  ( 5.999999999999998224, 0.000000000000000000, 5.000000000000000000 ) ) ;
#25228 = CARTESIAN_POINT ( 'NONE',  ( 111.5363082892543218, -5.992022692082500157, 45.00000000000000000 ) ) ;
#25229 = FACE_OUTER_BOUND ( 'NONE', #24183, .T. ) ;
#25230 = DIRECTION ( 'NONE',  ( 0.4528218681383056610, -0.8916010070293409751, 0.000000000000000000 ) ) ;
#25231 = EDGE_LOOP ( 'NONE', ( #15327, #26532, #23324, #27796 ) ) ;
#25232 = CARTESIAN_POINT ( 'NONE',  ( 157.4999999999998579, 88.33656210588026170, -45.00000000000000000 ) ) ;
#25233 = VERTEX_POINT ( 'NONE', #22448 ) ;
#25234 = EDGE_CURVE ( 'NONE', #24788, #8797, #9385, .T. ) ;
#25235 = CARTESIAN_POINT ( 'NONE',  ( 51.56615429303207065, 203.2034914284457159, -13.00000000000000000 ) ) ;
#25236 = EDGE_LOOP ( 'NONE', ( #19232, #23565, #24500, #26569, #16070 ) ) ;
#25237 = ORIENTED_EDGE ( 'NONE', *, *, #11489, .T. ) ;
#25238 = VECTOR ( 'NONE', #12370, 1000.000000000000000 ) ;
#25239 = VERTEX_POINT ( 'NONE', #24605 ) ;
#25240 = VECTOR ( 'NONE', #9501, 999.9999999999998863 ) ;
#25241 = ORIENTED_EDGE ( 'NONE', *, *, #11806, .F. ) ;
#25242 = ADVANCED_FACE ( 'NONE', ( #4910 ), #4770, .F. ) ;
#25243 = ORIENTED_EDGE ( 'NONE', *, *, #26940, .T. ) ;
#25244 = CARTESIAN_POINT ( 'NONE',  ( 158.0000000000005969, 150.7794997898028271, -45.00000000000000000 ) ) ;
#25245 = FACE_OUTER_BOUND ( 'NONE', #16110, .T. ) ;
#25246 = DIRECTION ( 'NONE',  ( -0.8660254037844359321, 0.5000000000000045519, 0.000000000000000000 ) ) ;
#25247 = EDGE_CURVE ( 'NONE', #21808, #12783, #13409, .T. ) ;
#25248 = EDGE_CURVE ( 'NONE', #8411, #5833, #22308, .T. ) ;
#25249 = ADVANCED_FACE ( 'NONE', ( #17849 ), #24886, .F. ) ;
#25250 = CARTESIAN_POINT ( 'NONE',  ( -96.46213353889478981, 134.5400755604871392, -15.50096989933989278 ) ) ;
#25251 = CARTESIAN_POINT ( 'NONE',  ( -208.1368626653883780, 75.14204529818155720, 39.73078884062161364 ) ) ;
#25252 = DIRECTION ( 'NONE',  ( 1.000000000000000000, -0.000000000000000000, -0.000000000000000000 ) ) ;
#25253 = CARTESIAN_POINT ( 'NONE',  ( -137.5457983441765464, 129.0117491753162255, -15.70601345937086535 ) ) ;
#25254 = AXIS2_PLACEMENT_3D ( 'NONE', #16050, #1086, #24942 ) ;
#25255 = DIRECTION ( 'NONE',  ( 1.000000000000000000, 0.000000000000000000, 0.000000000000000000 ) ) ;
#25256 = CARTESIAN_POINT ( 'NONE',  ( -203.7987795937083888, 92.08070442507484188, 29.54447684135760355 ) ) ;
#25257 = CARTESIAN_POINT ( 'NONE',  ( -235.6837214056122036, 120.7228219557777180, -15.00000000000000000 ) ) ;
#25258 = DIRECTION ( 'NONE',  ( 0.8916010070293783896, 0.4528218681382319422, 0.000000000000000000 ) ) ;
#25259 = CARTESIAN_POINT ( 'NONE',  ( 111.9999999999999574, 220.9999999999996874, -45.00000000000000000 ) ) ;
#25260 = EDGE_LOOP ( 'NONE', ( #4020, #7644, #25034, #20362 ) ) ;
#25261 = VECTOR ( 'NONE', #28270, 1000.000000000000000 ) ;
#25262 = CARTESIAN_POINT ( 'NONE',  ( 128.0812361363527998, 241.9574749595457774, 45.00000000000000000 ) ) ;
#25263 = DIRECTION ( 'NONE',  ( -0.000000000000000000, 1.000000000000000000, -1.387778780781445429E-16 ) ) ;
#25264 = PLANE ( 'NONE',  #22152 ) ;
#25266 = EDGE_LOOP ( 'NONE', ( #27665, #9739, #7187, #23402 ) ) ;
#25265 = ORIENTED_EDGE ( 'NONE', *, *, #27186, .T. ) ;
#25267 = CARTESIAN_POINT ( 'NONE',  ( -12.00299901279919723, 223.4254219457707222, 45.00000000000000000 ) ) ;
#25268 = ORIENTED_EDGE ( 'NONE', *, *, #19852, .T. ) ;
#25269 = ORIENTED_EDGE ( 'NONE', *, *, #17067, .T. ) ;
#25270 = ORIENTED_EDGE ( 'NONE', *, *, #2688, .T. ) ;
#25271 = ADVANCED_FACE ( 'NONE', ( #24750 ), #20290, .F. ) ;
#25272 = AXIS2_PLACEMENT_3D ( 'NONE', #14139, #7242, #16294 ) ;
#25273 = EDGE_LOOP ( 'NONE', ( #582, #24274, #20318, #3704 ) ) ;
#25274 = VERTEX_POINT ( 'NONE', #7224 ) ;
#25275 = DIRECTION ( 'NONE',  ( 0.000000000000000000, 0.000000000000000000, -1.000000000000000000 ) ) ;
#25276 = DIRECTION ( 'NONE',  ( -0.000000000000000000, 1.000000000000000000, -1.387778780781445429E-16 ) ) ;
#25277 = VECTOR ( 'NONE', #25993, 1000.000000000000000 ) ;
#25278 = EDGE_CURVE ( 'NONE', #13809, #4321, #4385, .T. ) ;
#25279 = LINE ( 'NONE', #3018, #4545 ) ;
#25280 = CARTESIAN_POINT ( 'NONE',  ( 107.0237911392832189, 245.0638502168177979, -31.95161221448068645 ) ) ;
#25281 = FACE_OUTER_BOUND ( 'NONE', #14931, .T. ) ;
#25282 = EDGE_CURVE ( 'NONE', #17145, #5416, #27035, .T. ) ;
#25283 = CARTESIAN_POINT ( 'NONE',  ( 113.0425250404538673, 226.9187638636466602, 45.00000000000000000 ) ) ;
#25284 = CARTESIAN_POINT ( 'NONE',  ( -190.0000000000000284, 59.99999999999995026, 98.28427124746191623 ) ) ;
#25285 = CARTESIAN_POINT ( 'NONE',  ( -220.8087078309937397, 71.35508338393960059, -21.10002476983576969 ) ) ;
#25286 = AXIS2_PLACEMENT_3D ( 'NONE', #1785, #25503, #10562 ) ;
#25287 = CARTESIAN_POINT ( 'NONE',  ( 110.0434296560979135, 203.3505179757799795, -150.6809294437985898 ) ) ;
#25288 = ADVANCED_BREP_SHAPE_REPRESENTATION ( '', ( #8854, #10637 ), #10190 ) ;
#25289 = CYLINDRICAL_SURFACE ( 'NONE', #15677, 30.00000000000000000 ) ;
#25290 = LINE ( 'NONE', #10213, #18473 ) ;
#25291 = EDGE_LOOP ( 'NONE', ( #26378, #8632 ) ) ;
#25292 = VECTOR ( 'NONE', #26070, 1000.000000000000000 ) ;
#25293 = LINE ( 'NONE', #3450, #2273 ) ;
#25294 = VECTOR ( 'NONE', #25968, 1000.000000000000114 ) ;
#25295 = DIRECTION ( 'NONE',  ( 0.000000000000000000, -1.000000000000000000, 0.000000000000000000 ) ) ;
#25296 = VERTEX_POINT ( 'NONE', #3040 ) ;
#25297 =( NAMED_UNIT ( * ) PLANE_ANGLE_UNIT ( ) SI_UNIT ( $, .RADIAN. ) );
#25298 = ORIENTED_EDGE ( 'NONE', *, *, #2472, .T. ) ;
#25299 = ORIENTED_EDGE ( 'NONE', *, *, #7391, .F. ) ;
#25300 = EDGE_CURVE ( 'NONE', #7477, #5352, #9236, .T. ) ;
#25301 = CARTESIAN_POINT ( 'NONE',  ( 89.77759941121971110, 81.13568025368125802, 100.0000000000000142 ) ) ;
#25302 = DIRECTION ( 'NONE',  ( 0.8916010070293383105, -0.4528218681383106015, 0.000000000000000000 ) ) ;
#25303 = ORIENTED_EDGE ( 'NONE', *, *, #21318, .T. ) ;
#25304 = ORIENTED_EDGE ( 'NONE', *, *, #3333, .T. ) ;
#25305 = CARTESIAN_POINT ( 'NONE',  ( 81.45493510941093973, 110.0000000000000142, -70.00000000034538061 ) ) ;
#25306 = AXIS2_PLACEMENT_3D ( 'NONE', #27750, #14561, #23316 ) ;
#25307 = CARTESIAN_POINT ( 'NONE',  ( 232.4999999999996305, 83.06687458711267880, 36.86484227207694175 ) ) ;
#25308 = DIRECTION ( 'NONE',  ( -0.000000000000000000, -0.000000000000000000, -1.000000000000000000 ) ) ;
#25309 = EDGE_LOOP ( 'NONE', ( #16694, #146 ) ) ;
#25310 = CARTESIAN_POINT ( 'NONE',  ( -228.3964932543056250, 90.87356368223484537, 15.41412920056914260 ) ) ;
#25311 = VERTEX_POINT ( 'NONE', #622 ) ;
#25312 = VECTOR ( 'NONE', #13408, 1000.000000000000000 ) ;
#25313 =( GEOMETRIC_REPRESENTATION_CONTEXT ( 3 ) GLOBAL_UNCERTAINTY_ASSIGNED_CONTEXT ( ( #840 ) ) GLOBAL_UNIT_ASSIGNED_CONTEXT ( ( #2464, #5197, #20426 ) ) REPRESENTATION_CONTEXT ( 'NONE', 'WORKASPACE' ) );
#25314 = CARTESIAN_POINT ( 'NONE',  ( 157.4999999999998579, 50.71843699327460797, -45.00000000000000000 ) ) ;
#25315 = AXIS2_PLACEMENT_3D ( 'NONE', #14324, #8419, #14894 ) ;
#25316 = EDGE_CURVE ( 'NONE', #23965, #16453, #8990, .T. ) ;
#25317 = ADVANCED_FACE ( 'NONE', ( #760 ), #24313, .F. ) ;
#25318 = DIRECTION ( 'NONE',  ( 0.4528218681373508692, -0.8916010070298259205, 0.000000000000000000 ) ) ;
#25319 = LINE ( 'NONE', #20448, #19465 ) ;
#25320 = CARTESIAN_POINT ( 'NONE',  ( -290.0000000000001137, -220.0000000000000853, 60.00000000000002842 ) ) ;
#25321 = DIRECTION ( 'NONE',  ( 1.000000000000000000, 4.625929269271485914E-16, 0.000000000000000000 ) ) ;
#25322 = CARTESIAN_POINT ( 'NONE',  ( -231.9378824387731299, 93.53122965655670384, 12.99999999999999822 ) ) ;
#25323 = CARTESIAN_POINT ( 'NONE',  ( -180.4068668408075666, 109.4706979435998306, -30.97813022004903516 ) ) ;
#25324 = ORIENTED_EDGE ( 'NONE', *, *, #13405, .F. ) ;
#25325 = LINE ( 'NONE', #6064, #15537 ) ;
#25326 = LINE ( 'NONE', #13764, #963 ) ;
#25327 = PLANE ( 'NONE',  #25306 ) ;
#25328 = LINE ( 'NONE', #5652, #660 ) ;
#25329 = ORIENTED_EDGE ( 'NONE', *, *, #12091, .T. ) ;
#25330 = EDGE_CURVE ( 'NONE', #1070, #26295, #3934, .T. ) ;
#25331 = CARTESIAN_POINT ( 'NONE',  ( 157.4999999999996305, 286.4586876989355915, 45.00000000000000000 ) ) ;
#25332 = ORIENTED_EDGE ( 'NONE', *, *, #21905, .T. ) ;
#25333 = EDGE_CURVE ( 'NONE', #9426, #761, #15158, .T. ) ;
#25334 = TOROIDAL_SURFACE ( 'NONE', #1030, 60.00000000000000000, 30.00000000000000000 ) ;
#25335 = DIRECTION ( 'NONE',  ( -0.000000000000000000, 1.000000000000000000, -1.387778780781445429E-16 ) ) ;
#25336 = FACE_OUTER_BOUND ( 'NONE', #23077, .T. ) ;
#25337 = PLANE ( 'NONE',  #243 ) ;
#25338 = ORIENTED_EDGE ( 'NONE', *, *, #23982, .F. ) ;
#25339 = LINE ( 'NONE', #4056, #19388 ) ;
#25340 = AXIS2_PLACEMENT_3D ( 'NONE', #6753, #10931, #4451 ) ;
#25341 = ORIENTED_EDGE ( 'NONE', *, *, #2643, .F. ) ;
#25342 = VECTOR ( 'NONE', #25410, 1000.000000000000000 ) ;
#25343 = DIRECTION ( 'NONE',  ( 1.000000000000000000, 0.000000000000000000, 0.000000000000000000 ) ) ;
#25344 = CARTESIAN_POINT ( 'NONE',  ( 157.4999999999998579, 53.22631200078164682, 45.00000000000000000 ) ) ;
#25345 = ORIENTED_EDGE ( 'NONE', *, *, #20147, .T. ) ;
#25346 = EDGE_LOOP ( 'NONE', ( #18243, #7724, #9914, #20193 ) ) ;
#25347 = CARTESIAN_POINT ( 'NONE',  ( 25.90578987075423001, -14.95671475544977724, -45.00000000000000000 ) ) ;
#25348 = ORIENTED_EDGE ( 'NONE', *, *, #15362, .T. ) ;
#25349 = ORIENTED_EDGE ( 'NONE', *, *, #19028, .F. ) ;
#25350 = VERTEX_POINT ( 'NONE', #16551 ) ;
#25351 = B_SPLINE_CURVE_WITH_KNOTS ( 'NONE', 3,
 ( #22757, #11845, #5499, #491, #9252, #9403, #16014, #20590, #24767, #5074, #13864, #17125 ),
 .UNSPECIFIED., .F., .F.,
 ( 4, 2, 2, 2, 2, 4 ),
 ( 0.000000000000000000, 0.003876131231190137454, 0.007752262462380274909, 0.009690328077975263188, 0.01162839369357025233, 0.01550452492476005022 ),
 .UNSPECIFIED. ) ;
#25352 = AXIS2_PLACEMENT_3D ( 'NONE', #25307, #10369, #21562 ) ;
#25353 = DIRECTION ( 'NONE',  ( 0.000000000000000000, 0.000000000000000000, 1.000000000000000000 ) ) ;
#25354 = ADVANCED_FACE ( 'NONE', ( #5624 ), #5480, .T. ) ;
#25355 = EDGE_CURVE ( 'NONE', #15447, #3282, #27308, .T. ) ;
#25356 = VECTOR ( 'NONE', #5160, 1000.000000000000000 ) ;
#25357 = CARTESIAN_POINT ( 'NONE',  ( 282.4999999999996589, 19.41075299063184900, 87.99671038392668265 ) ) ;
#25358 = CARTESIAN_POINT ( 'NONE',  ( 158.0000000000005400, 155.7952498048169048, 45.00000000000000000 ) ) ;
#25359 = AXIS2_PLACEMENT_3D ( 'NONE', #14382, #9926, #25143 ) ;
#25360 = VECTOR ( 'NONE', #27106, 1000.000000000000000 ) ;
#25361 = LINE ( 'NONE', #8403, #26166 ) ;
#25362 = DIRECTION ( 'NONE',  ( 0.9960550913260672878, 1.086714821493793968E-17, 0.08873699929240064233 ) ) ;
#25363 = DIRECTION ( 'NONE',  ( 1.000000000000000000, -0.000000000000000000, -0.000000000000000000 ) ) ;
#25364 = PLANE ( 'NONE',  #1221 ) ;
#25365 = CARTESIAN_POINT ( 'NONE',  ( -279.1278187736259611, -165.0000000000001421, 106.1966075482099541 ) ) ;
#25366 = DIRECTION ( 'NONE',  ( -4.540956701092242152E-16, -1.000000000000000000, -0.000000000000000000 ) ) ;
#25367 = DIRECTION ( 'NONE',  ( -2.139922160430261846E-32, 1.387778780781445429E-16, 1.000000000000000000 ) ) ;
#25368 = VERTEX_POINT ( 'NONE', #18698 ) ;
#25369 = CARTESIAN_POINT ( 'NONE',  ( 157.4999999999998579, 148.5255622860493077, -45.00000000000000000 ) ) ;
#25370 = CARTESIAN_POINT ( 'NONE',  ( 109.9999999999999005, 260.0000000000000000, -45.00000000000000000 ) ) ;
#25371 = CARTESIAN_POINT ( 'NONE',  ( 24.59638288546416973, 86.21496700725640494, 99.35042210466092172 ) ) ;
#25372 = CARTESIAN_POINT ( 'NONE',  ( 158.0000000000005400, 153.7952498048169048, 45.00000000000000000 ) ) ;
#25373 = DIRECTION ( 'NONE',  ( -1.000000000000000000, -2.312964634635742957E-16, 0.000000000000000000 ) ) ;
#25374 = EDGE_LOOP ( 'NONE', ( #3216, #3363, #9522, #4130 ) ) ;
#25375 = EDGE_CURVE ( 'NONE', #23503, #19001, #12251, .T. ) ;
#25376 = VECTOR ( 'NONE', #18709, 1000.000000000000000 ) ;
#25377 = EDGE_CURVE ( 'NONE', #12779, #7297, #8520, .T. ) ;
#25378 = AXIS2_PLACEMENT_3D ( 'NONE', #5512, #25335, #9831 ) ;
#25379 = CARTESIAN_POINT ( 'NONE',  ( -260.0000000000001137, -167.0819201924624622, -104.9999999999998721 ) ) ;
#25380 = VERTEX_POINT ( 'NONE', #5901 ) ;
#25381 = DIRECTION ( 'NONE',  ( 0.000000000000000000, 0.000000000000000000, -1.000000000000000000 ) ) ;
#25382 = ORIENTED_EDGE ( 'NONE', *, *, #2793, .T. ) ;
#25383 = EDGE_CURVE ( 'NONE', #28122, #19128, #1449, .T. ) ;
#25384 = VECTOR ( 'NONE', #23674, 1000.000000000000114 ) ;
#25385 = ORIENTED_EDGE ( 'NONE', *, *, #9977, .F. ) ;
#25386 = ORIENTED_EDGE ( 'NONE', *, *, #5164, .F. ) ;
#25387 = ORIENTED_EDGE ( 'NONE', *, *, #26222, .T. ) ;
#25388 = DIRECTION ( 'NONE',  ( -0.000000000000000000, 1.000000000000000000, -1.387778780781445429E-16 ) ) ;
#25389 = CARTESIAN_POINT ( 'NONE',  ( 158.0000000000008242, 126.2086247222394206, -45.00000000000000000 ) ) ;
#25390 = DIRECTION ( 'NONE',  ( 0.000000000000000000, 0.000000000000000000, 1.000000000000000000 ) ) ;
#25391 = CARTESIAN_POINT ( 'NONE',  ( 157.9999999999996305, 288.7126252026890256, -45.00000000000000000 ) ) ;
#25392 = TOROIDAL_SURFACE ( 'NONE', #17596, 11.00000000000001066, 1.000000000000000000 ) ;
#25393 = CARTESIAN_POINT ( 'NONE',  ( -208.8418814728804023, 74.65865074066952900, 37.27912060900214186 ) ) ;
#25394 = LINE ( 'NONE', #8012, #19663 ) ;
#25395 = CARTESIAN_POINT ( 'NONE',  ( -152.9354250843960585, 123.6290117556221162, -18.69239437641641999 ) ) ;
#25396 = VECTOR ( 'NONE', #13851, 1000.000000000000000 ) ;
#25397 = DIRECTION ( 'NONE',  ( -0.000000000000000000, 0.000000000000000000, -1.000000000000000000 ) ) ;
#25398 = LINE ( 'NONE', #10034, #25940 ) ;
#25399 = VECTOR ( 'NONE', #19885, 1000.000000000000114 ) ;
#25400 = DIRECTION ( 'NONE',  ( -0.000000000000000000, 0.000000000000000000, -1.000000000000000000 ) ) ;
#25401 = CARTESIAN_POINT ( 'NONE',  ( 157.9999999999998010, 239.0630000600560550, -45.00000000000000000 ) ) ;
#25402 = CARTESIAN_POINT ( 'NONE',  ( 157.9999999999998295, 224.0157500150140208, -45.00000000000000000 ) ) ;
#25403 = VERTEX_POINT ( 'NONE', #9804 ) ;
#25404 = CARTESIAN_POINT ( 'NONE',  ( -175.0000000000000000, -120.0250000000001904, -69.99999999999998579 ) ) ;
#25405 = CARTESIAN_POINT ( 'NONE',  ( -203.2481855153402250, 92.57460631283319685, 29.78692811926998729 ) ) ;
#25406 = EDGE_CURVE ( 'NONE', #606, #18799, #28225, .T. ) ;
#25408 = ORIENTED_EDGE ( 'NONE', *, *, #7391, .T. ) ;
#25407 = ORIENTED_EDGE ( 'NONE', *, *, #206, .F. ) ;
#25409 = EDGE_CURVE ( 'NONE', #27440, #5806, #3457, .T. ) ;
#25410 = DIRECTION ( 'NONE',  ( 0.000000000000000000, -1.000000000000000000, 0.000000000000000000 ) ) ;
#25411 = EDGE_CURVE ( 'NONE', #5026, #3340, #27582, .T. ) ;
#25412 = ORIENTED_EDGE ( 'NONE', *, *, #8807, .F. ) ;
#25413 = ORIENTED_EDGE ( 'NONE', *, *, #24507, .T. ) ;
#25414 = VECTOR ( 'NONE', #13643, 1000.000000000000000 ) ;
#25415 = ORIENTED_EDGE ( 'NONE', *, *, #7973, .T. ) ;
#25416 = VERTEX_POINT ( 'NONE', #18560 ) ;
#25417 = VECTOR ( 'NONE', #9078, 1000.000000000000000 ) ;
#25418 = ORIENTED_EDGE ( 'NONE', *, *, #26538, .T. ) ;
#25419 = ORIENTED_EDGE ( 'NONE', *, *, #9125, .T. ) ;
#25420 = CARTESIAN_POINT ( 'NONE',  ( 115.1711027725237955, 217.3894761555985156, 45.00000000000000000 ) ) ;
#25421 = FACE_BOUND ( 'NONE', #9238, .T. ) ;
#25422 = CARTESIAN_POINT ( 'NONE',  ( 108.4328758917250468, 248.8772442435372056, -35.32571066851171082 ) ) ;
#25423 = CARTESIAN_POINT ( 'NONE',  ( 5.538391900817774882, 137.3871724827027947, -15.09218160842566370 ) ) ;
#25424 = CARTESIAN_POINT ( 'NONE',  ( 158.0000000000005969, 150.7794997898028271, 45.00000000000000000 ) ) ;
#25425 = DIRECTION ( 'NONE',  ( -0.000000000000000000, 0.000000000000000000, 1.000000000000000000 ) ) ;
#25426 = LINE ( 'NONE', #1013, #13457 ) ;
#25427 = CIRCLE ( 'NONE', #13069, 35.18636678425507114 ) ;
#25428 = EDGE_CURVE ( 'NONE', #15348, #3825, #23292, .T. ) ;
#25429 = CARTESIAN_POINT ( 'NONE',  ( 179.9999999999999147, -150.0000000000000284, 100.0000000000000142 ) ) ;
#25430 = CARTESIAN_POINT ( 'NONE',  ( 3.469446951953617344E-15, -40.00000000000003553, -70.00000000000001421 ) ) ;
#25431 = FACE_OUTER_BOUND ( 'NONE', #17142, .T. ) ;
#25432 = CARTESIAN_POINT ( 'NONE',  ( 157.4999999999997442, 251.3484375938375024, -45.00000000000000000 ) ) ;
#25433 = AXIS2_PLACEMENT_3D ( 'NONE', #11470, #18353, #397 ) ;
#25434 = ORIENTED_EDGE ( 'NONE', *, *, #8265, .F. ) ;
#25435 = CARTESIAN_POINT ( 'NONE',  ( -195.0245959749996132, 99.69668914553523109, 31.69045126054473371 ) ) ;
#25436 = EDGE_CURVE ( 'NONE', #20816, #16250, #11967, .T. ) ;
#25437 = EDGE_CURVE ( 'NONE', #28117, #24036, #10224, .T. ) ;
#25438 = CARTESIAN_POINT ( 'NONE',  ( -12.24491960465745599, -23.01420295945612082, 80.00000000000001421 ) ) ;
#25439 = ORIENTED_EDGE ( 'NONE', *, *, #924, .T. ) ;
#25440 = EDGE_LOOP ( 'NONE', ( #24426, #18808, #18279, #22326 ) ) ;
#25441 = ORIENTED_EDGE ( 'NONE', *, *, #13823, .T. ) ;
#25442 = CARTESIAN_POINT ( 'NONE',  ( 84.91648909974954051, 110.3843228243387102, 100.0000000000000142 ) ) ;
#25443 = CARTESIAN_POINT ( 'NONE',  ( 1.633516369018864101, 1.249999999999999556, 7.514731128045609942 ) ) ;
#25444 = ORIENTED_EDGE ( 'NONE', *, *, #16660, .T. ) ;
#25445 = CIRCLE ( 'NONE', #13085, 5.000000000000004441 ) ;
#25446 = VERTEX_POINT ( 'NONE', #16829 ) ;
#25447 = PLANE ( 'NONE',  #2147 ) ;
#25448 = B_SPLINE_CURVE_WITH_KNOTS ( 'NONE', 3,
 ( #8490, #8918, #12952, #8634, #17389, #2156, #26003, #26425, #4167 ),
 .UNSPECIFIED., .F., .F.,
 ( 4, 2, 1, 2, 4 ),
 ( 0.000000000000000000, 0.003850132855190854363, 0.007700265710381708727, 0.01155039856557256266, 0.01540053142076341745 ),
 .UNSPECIFIED. ) ;
#25449 = DIRECTION ( 'NONE',  ( -0.000000000000000000, -1.000000000000000000, -0.000000000000000000 ) ) ;
#25450 = CARTESIAN_POINT ( 'NONE',  ( -42.53273978471831640, 130.9733465240572627, -15.00000000000000000 ) ) ;
#25451 = ORIENTED_EDGE ( 'NONE', *, *, #11403, .T. ) ;
#25452 = ORIENTED_EDGE ( 'NONE', *, *, #7974, .T. ) ;
#25453 = AXIS2_PLACEMENT_3D ( 'NONE', #8097, #19292, #26177 ) ;
#25454 = DIRECTION ( 'NONE',  ( -0.000000000000000000, -0.000000000000000000, -1.000000000000000000 ) ) ;
#25455 = CARTESIAN_POINT ( 'NONE',  ( 157.4999999999996874, 268.9035626463865469, 45.00000000000000000 ) ) ;
#25456 = DIRECTION ( 'NONE',  ( 0.8916010070293783896, -0.4528218681382319422, 0.000000000000000000 ) ) ;
#25457 = EDGE_CURVE ( 'NONE', #1534, #6404, #3740, .T. ) ;
#25458 = CARTESIAN_POINT ( 'NONE',  ( -210.0000000000000568, -220.0000000000000853, 110.0000000000000284 ) ) ;
#25459 = CARTESIAN_POINT ( 'NONE',  ( 79.99999999999992895, 110.0000000000000000, -45.00000000000000000 ) ) ;
#25460 = LINE ( 'NONE', #5782, #26186 ) ;
#25461 = CARTESIAN_POINT ( 'NONE',  ( 161.7277574978466816, 206.3741923490296131, -150.7960377432351891 ) ) ;
#25462 = EDGE_CURVE ( 'NONE', #1874, #12868, #20853, .T. ) ;
#25463 = ORIENTED_EDGE ( 'NONE', *, *, #27105, .F. ) ;
#25464 = CARTESIAN_POINT ( 'NONE',  ( 157.4999999999996305, 283.9508126914284958, 45.00000000000000000 ) ) ;
#25465 = VECTOR ( 'NONE', #4529, 1000.000000000000000 ) ;
#25466 = CARTESIAN_POINT ( 'NONE',  ( 232.4999999999996305, 133.0668745871126930, -42.86484227207692044 ) ) ;
#25467 = FACE_OUTER_BOUND ( 'NONE', #21636, .T. ) ;
#25468 = CYLINDRICAL_SURFACE ( 'NONE', #13518, 75.00000000000002842 ) ;
#25469 = ORIENTED_EDGE ( 'NONE', *, *, #27074, .T. ) ;
#25470 = VECTOR ( 'NONE', #26985, 1000.000000000000000 ) ;
#25471 = CARTESIAN_POINT ( 'NONE',  ( 109.9999999999999005, 3.816391647148972452E-14, -70.00000000000001421 ) ) ;
#25472 = ORIENTED_EDGE ( 'NONE', *, *, #20597, .T. ) ;
#25473 = EDGE_CURVE ( 'NONE', #27032, #2768, #20708, .T. ) ;
#25474 = CYLINDRICAL_SURFACE ( 'NONE', #1969, 58.90601976618767566 ) ;
#25475 = DIRECTION ( 'NONE',  ( 0.000000000000000000, 0.000000000000000000, -1.000000000000000000 ) ) ;
#25476 = CARTESIAN_POINT ( 'NONE',  ( 217.4999999999996305, -5.589247009368160768, 100.0000000000000142 ) ) ;
#25477 = ORIENTED_EDGE ( 'NONE', *, *, #2169, .T. ) ;
#25478 = CARTESIAN_POINT ( 'NONE',  ( -277.2150368962633706, -237.2150368962634559, -104.9999999999998295 ) ) ;
#25479 = DIRECTION ( 'NONE',  ( -0.000000000000000000, -0.000000000000000000, -1.000000000000000000 ) ) ;
#25480 = VECTOR ( 'NONE', #19114, 1000.000000000000000 ) ;
#25481 = ORIENTED_EDGE ( 'NONE', *, *, #23327, .T. ) ;
#25482 = EDGE_CURVE ( 'NONE', #19998, #2218, #14980, .T. ) ;
#25483 = CARTESIAN_POINT ( 'NONE',  ( 134.9999999999998579, 220.0000000000000284, -90.00000000000002842 ) ) ;
#25484 = DIRECTION ( 'NONE',  ( -0.8916010070299977830, 0.4528218681370124177, 0.000000000000000000 ) ) ;
#25485 = ORIENTED_EDGE ( 'NONE', *, *, #15793, .F. ) ;
#25486 = ORIENTED_EDGE ( 'NONE', *, *, #19633, .T. ) ;
#25487 = CARTESIAN_POINT ( 'NONE',  ( 0.000000000000000000, 1.249999999999999556, 6.997769477110050929 ) ) ;
#25488 = VERTEX_POINT ( 'NONE', #27174 ) ;
#25489 = VECTOR ( 'NONE', #5215, 1000.000000000000000 ) ;
#25490 = ORIENTED_EDGE ( 'NONE', *, *, #27975, .F. ) ;
#25491 = VERTEX_POINT ( 'NONE', #7511 ) ;
#25492 = VECTOR ( 'NONE', #5682, 1000.000000000000000 ) ;
#25493 = AXIS2_PLACEMENT_3D ( 'NONE', #25344, #12290, #25484 ) ;
#25494 = ADVANCED_FACE ( 'NONE', ( #16278 ), #25031, .F. ) ;
#25495 = CARTESIAN_POINT ( 'NONE',  ( 9.999999999999738876, -50.00000000000004263, 110.0000000000000284 ) ) ;
#25496 = CARTESIAN_POINT ( 'NONE',  ( -225.9729034214362571, 132.4331356209112300, 12.99353264133693919 ) ) ;
#25497 = LINE ( 'NONE', #5814, #22495 ) ;
#25498 = DIRECTION ( 'NONE',  ( -0.000000000000000000, -0.000000000000000000, -1.000000000000000000 ) ) ;
#25499 = PLANE ( 'NONE',  #5760 ) ;
#25500 = EDGE_CURVE ( 'NONE', #20823, #16820, #8491, .T. ) ;
#25501 = CARTESIAN_POINT ( 'NONE',  ( -221.7690971916800322, 71.47334710437645811, -20.39711061091116662 ) ) ;
#25502 = CARTESIAN_POINT ( 'NONE',  ( 0.3651377029009472142, 1.249999999999999556, -7.402212548643259282 ) ) ;
#25503 = DIRECTION ( 'NONE',  ( -0.000000000000000000, -0.000000000000000000, 1.000000000000000000 ) ) ;
#25504 = DIRECTION ( 'NONE',  ( 0.8916010070317489378, -0.4528218681335642315, 0.000000000000000000 ) ) ;
#25505 = DIRECTION ( 'NONE',  ( -0.7440215159219069063, -0.6681556583950086781, 0.000000000000000000 ) ) ;
#25506 = EDGE_LOOP ( 'NONE', ( #19973, #16739, #24158, #12607 ) ) ;
#25507 = LINE ( 'NONE', #5691, #13248 ) ;
#25508 = CARTESIAN_POINT ( 'NONE',  ( 157.9999999999998010, 236.0472500450420341, 45.00000000000000000 ) ) ;
#25509 = CARTESIAN_POINT ( 'NONE',  ( 157.4999999999998579, 103.3838121509225090, -45.00000000000000000 ) ) ;
#25510 = SURFACE_SIDE_STYLE ('',( #16759 ) ) ;
#25511 = CYLINDRICAL_SURFACE ( 'NONE', #1015, 30.00000000000000000 ) ;
#25512 = ORIENTED_EDGE ( 'NONE', *, *, #8204, .T. ) ;
#25513 = VECTOR ( 'NONE', #12814, 1000.000000000000000 ) ;
#25514 = EDGE_CURVE ( 'NONE', #27280, #20930, #28007, .T. ) ;
#25515 = ADVANCED_FACE ( 'NONE', ( #26004 ), #10792, .F. ) ;
#25516 = CARTESIAN_POINT ( 'NONE',  ( -232.2365570322886299, 76.71063732366134502, 15.57345046155156432 ) ) ;
#25517 = ORIENTED_EDGE ( 'NONE', *, *, #7986, .F. ) ;
#25518 = CARTESIAN_POINT ( 'NONE',  ( 134.9999999999998579, 220.0000000000000284, 45.00000000000000000 ) ) ;
#25519 = ORIENTED_EDGE ( 'NONE', *, *, #10483, .F. ) ;
#25520 = ORIENTED_EDGE ( 'NONE', *, *, #21408, .T. ) ;
#25521 = CARTESIAN_POINT ( 'NONE',  ( -47.46858701631881416, 132.2250854490906420, 14.48589841498654174 ) ) ;
#25522 = ORIENTED_EDGE ( 'NONE', *, *, #16311, .T. ) ;
#25523 = ORIENTED_EDGE ( 'NONE', *, *, #18083, .T. ) ;
#25524 = CARTESIAN_POINT ( 'NONE',  ( 112.8630565061745017, 215.9427151076712619, 97.00605251950267416 ) ) ;
#25525 = EDGE_CURVE ( 'NONE', #1333, #13440, #3955, .T. ) ;
#25526 = DIRECTION ( 'NONE',  ( -0.000000000000000000, -0.000000000000000000, -1.000000000000000000 ) ) ;
#25527 = CARTESIAN_POINT ( 'NONE',  ( -211.8229433495291971, -220.0000000000000853, -93.01810040011434921 ) ) ;
#25528 = CARTESIAN_POINT ( 'NONE',  ( -152.6794942072440904, 123.7315770332490956, -19.76807053014819004 ) ) ;
#25529 = EDGE_CURVE ( 'NONE', #12360, #7085, #1729, .T. ) ;
#25530 = DIRECTION ( 'NONE',  ( 1.000000000000000000, 0.000000000000000000, 0.000000000000000000 ) ) ;
#25531 = DIRECTION ( 'NONE',  ( 0.000000000000000000, -0.000000000000000000, 1.000000000000000000 ) ) ;
#25532 = DIRECTION ( 'NONE',  ( 0.7082136108520787898, 0.7059982162894324897, -0.000000000000000000 ) ) ;
#25533 = CARTESIAN_POINT ( 'NONE',  ( 129.3169142913460234, 249.4568486868007540, -143.0657854549350532 ) ) ;
#25534 = CARTESIAN_POINT ( 'NONE',  ( -143.6428522700808230, 20.24192588826928585, 83.00000000000001421 ) ) ;
#25535 = EDGE_CURVE ( 'NONE', #25488, #6227, #6325, .T. ) ;
#25536 = CARTESIAN_POINT ( 'NONE',  ( 28.57744295357075259, -14.51376905457599342, -45.00000000000000000 ) ) ;
#25537 = LINE ( 'NONE', #3694, #19644 ) ;
#25538 = DIRECTION ( 'NONE',  ( -0.2588190451025321748, -0.9659258262890652036, 0.000000000000000000 ) ) ;
#25539 = ORIENTED_EDGE ( 'NONE', *, *, #6193, .F. ) ;
#25540 = CARTESIAN_POINT ( 'NONE',  ( 93.99999999999985789, 171.5103103742661972, -105.0000000000000284 ) ) ;
#25541 = LINE ( 'NONE', #19222, #15693 ) ;
#25543 = EDGE_LOOP ( 'NONE', ( #14577, #11220, #18294, #18417 ) ) ;
#25542 = ORIENTED_EDGE ( 'NONE', *, *, #7217, .T. ) ;
#25544 = CARTESIAN_POINT ( 'NONE',  ( -12.00299901279919723, 223.4254219457707222, 45.00000000000000000 ) ) ;
#25545 = VERTEX_POINT ( 'NONE', #14826 ) ;
#25546 = ORIENTED_EDGE ( 'NONE', *, *, #15833, .T. ) ;
#25547 = ORIENTED_EDGE ( 'NONE', *, *, #20675, .T. ) ;
#25548 = ORIENTED_EDGE ( 'NONE', *, *, #18706, .T. ) ;
#25549 = ORIENTED_EDGE ( 'NONE', *, *, #25110, .F. ) ;
#25550 = ORIENTED_EDGE ( 'NONE', *, *, #17273, .T. ) ;
#25551 = DIRECTION ( 'NONE',  ( -0.6782242722910949428, -0.7348549764921067373, 0.000000000000000000 ) ) ;
#25552 = DIRECTION ( 'NONE',  ( -0.000000000000000000, -1.000000000000000000, -0.000000000000000000 ) ) ;
#25553 = EDGE_CURVE ( 'NONE', #17961, #13726, #17529, .T. ) ;
#25554 = CARTESIAN_POINT ( 'NONE',  ( 109.9984815155424656, 259.5975204907896909, -44.65144252145412906 ) ) ;
#25555 = ADVANCED_FACE ( 'NONE', ( #21705 ), #23577, .F. ) ;
#25556 = PLANE ( 'NONE',  #22500 ) ;
#25557 = CARTESIAN_POINT ( 'NONE',  ( 158.0000000000005116, 160.8109998198309825, 45.00000000000000000 ) ) ;
#25558 = DIRECTION ( 'NONE',  ( 0.000000000000000000, 0.000000000000000000, -1.000000000000000000 ) ) ;
#25559 = VECTOR ( 'NONE', #25696, 1000.000000000000114 ) ;
#25560 = CARTESIAN_POINT ( 'NONE',  ( -207.5044420441007276, 75.59897387903043864, -45.00000000000000000 ) ) ;
#25561 = CARTESIAN_POINT ( 'NONE',  ( 112.4076948732478911, 200.2619365998405954, -143.4419542882358201 ) ) ;
#25562 = DIRECTION ( 'NONE',  ( -0.8916010070294396739, 0.4528218681381114274, 0.000000000000000000 ) ) ;
#25563 = CARTESIAN_POINT ( 'NONE',  ( -76.25760768171836901, 154.8982798170083299, 15.00000000000000000 ) ) ;
#25564 = ORIENTED_EDGE ( 'NONE', *, *, #1640, .F. ) ;
#25565 = CARTESIAN_POINT ( 'NONE',  ( -237.3870311360069536, 121.7710280244218950, 13.00000000000000000 ) ) ;
#25566 = EDGE_CURVE ( 'NONE', #21412, #18321, #26294, .T. ) ;
#25567 = CARTESIAN_POINT ( 'NONE',  ( -261.1919288306252724, -171.9377729149742038, -109.9999999999998721 ) ) ;
#25568 = ORIENTED_EDGE ( 'NONE', *, *, #15869, .T. ) ;
#25569 = SHAPE_DEFINITION_REPRESENTATION ( #4067, #14145 ) ;
#25570 = ORIENTED_EDGE ( 'NONE', *, *, #15765, .F. ) ;
#25571 = ORIENTED_EDGE ( 'NONE', *, *, #2049, .F. ) ;
#25572 = TOROIDAL_SURFACE ( 'NONE', #15990, 34.99999999999999289, 5.000000000000000000 ) ;
#25573 = PLANE ( 'NONE',  #13389 ) ;
#25574 = EDGE_CURVE ( 'NONE', #24468, #16686, #21851, .T. ) ;
#25575 = CARTESIAN_POINT ( 'NONE',  ( 158.0000000000011084, 98.62199963966197913, 45.00000000000000000 ) ) ;
#25576 = ORIENTED_EDGE ( 'NONE', *, *, #26398, .F. ) ;
#25577 = ORIENTED_EDGE ( 'NONE', *, *, #436, .T. ) ;
#25578 = DIRECTION ( 'NONE',  ( 1.321694076934710155E-16, -1.000000000000000000, 0.000000000000000000 ) ) ;
#25579 = CARTESIAN_POINT ( 'NONE',  ( 109.2201559107103037, 251.9988677676353177, 38.05717760203712174 ) ) ;
#25580 = CARTESIAN_POINT ( 'NONE',  ( -208.4194785928031877, -215.2563777467642296, 60.00000000000002132 ) ) ;
#25581 = ORIENTED_EDGE ( 'NONE', *, *, #24112, .F. ) ;
#25582 = ADVANCED_FACE ( 'NONE', ( #2157 ), #2017, .F. ) ;
#25583 = CARTESIAN_POINT ( 'NONE',  ( 176.5942101292460222, 101.9567147554491271, -45.00000000000000000 ) ) ;
#25584 = EDGE_LOOP ( 'NONE', ( #14435, #4170, #27547, #1699 ) ) ;
#25585 = CARTESIAN_POINT ( 'NONE',  ( 134.9999999999998579, 220.0000000000000284, -99.00000000000001421 ) ) ;
#25586 = EDGE_CURVE ( 'NONE', #28150, #7922, #24152, .T. ) ;
#25587 = EDGE_CURVE ( 'NONE', #27002, #2675, #17262, .T. ) ;
#25588 = CARTESIAN_POINT ( 'NONE',  ( 33.10302365956999182, 203.2034914284457159, -15.00000000000000000 ) ) ;
#25589 = CARTESIAN_POINT ( 'NONE',  ( -55.40193461144291831, 169.7519813918499665, 45.00000000000000000 ) ) ;
#25590 = DIRECTION ( 'NONE',  ( -0.000000000000000000, -0.000000000000000000, -1.000000000000000000 ) ) ;
#25591 = PLANE ( 'NONE',  #19622 ) ;
#25592 = CARTESIAN_POINT ( 'NONE',  ( 0.000000000000000000, 0.000000000000000000, -100.0000000000000142 ) ) ;
#25593 = CARTESIAN_POINT ( 'NONE',  ( 163.4557797152162095, 210.4990210588524064, -144.6008566625276615 ) ) ;
#25594 = CONICAL_SURFACE ( 'NONE', #16008, 6.025000000000002132, 0.7853981633974482790 ) ;
#25595 = ORIENTED_EDGE ( 'NONE', *, *, #7673, .F. ) ;
#25596 = DIRECTION ( 'NONE',  ( 1.000000000000000000, -0.000000000000000000, -0.000000000000000000 ) ) ;
#25597 = VECTOR ( 'NONE', #9546, 1000.000000000000227 ) ;
#25598 = CARTESIAN_POINT ( 'NONE',  ( 65.00000000000000000, -120.0000000000000995, -64.00000000000000000 ) ) ;
#25599 = DIRECTION ( 'NONE',  ( -0.000000000000000000, -0.000000000000000000, -1.000000000000000000 ) ) ;
#25600 = DIRECTION ( 'NONE',  ( -0.000000000000000000, 1.000000000000000000, -1.387778780781445429E-16 ) ) ;
#25601 = ORIENTED_EDGE ( 'NONE', *, *, #18693, .F. ) ;
#25602 = CARTESIAN_POINT ( 'NONE',  ( 157.9999999999998579, 219.0000000000000284, -45.00000000000000000 ) ) ;
#25603 = ORIENTED_EDGE ( 'NONE', *, *, #23557, .F. ) ;
#25604 =( REPRESENTATION_RELATIONSHIP ('NONE','NONE', #11963, #22013 ) REPRESENTATION_RELATIONSHIP_WITH_TRANSFORMATION ( #21268 )SHAPE_REPRESENTATION_RELATIONSHIP( ) );
#25605 = CARTESIAN_POINT ( 'NONE',  ( 0.000000000000000000, 0.000000000000000000, -110.0000000000000284 ) ) ;
#25606 = FACE_OUTER_BOUND ( 'NONE', #590, .T. ) ;
#25607 = DIRECTION ( 'NONE',  ( 0.8660254037844432595, 0.4999999999999919509, -0.000000000000000000 ) ) ;
#25608 = EDGE_LOOP ( 'NONE', ( #5619, #15294, #22704, #723 ) ) ;
#25609 = LINE ( 'NONE', #3214, #22559 ) ;
#25610 = DIRECTION ( 'NONE',  ( 1.000000000000000000, 8.542487643439285958E-16, 0.000000000000000000 ) ) ;
#25611 = ORIENTED_EDGE ( 'NONE', *, *, #24535, .F. ) ;
#25612 = CARTESIAN_POINT ( 'NONE',  ( -148.7496381368905247, 124.1794587942970907, 19.49431050908225060 ) ) ;
#25613 = AXIS2_PLACEMENT_3D ( 'NONE', #16887, #27791, #19322 ) ;
#25614 = PLANE ( 'NONE',  #25493 ) ;
#25615 = ORIENTED_EDGE ( 'NONE', *, *, #26008, .T. ) ;
#25616 = VERTEX_POINT ( 'NONE', #19262 ) ;
#25617 = CARTESIAN_POINT ( 'NONE',  ( -210.0000000000000853, -212.3568517473289887, -110.0000000000000568 ) ) ;
#25618 = ADVANCED_FACE ( 'NONE', ( #2293 ), #8350, .F. ) ;
#25619 = ORIENTED_EDGE ( 'NONE', *, *, #25437, .T. ) ;
#25620 = EDGE_CURVE ( 'NONE', #27414, #16958, #25866, .T. ) ;
#25621 = PRODUCT_DEFINITION_SHAPE ( 'NONE', 'NONE',  #28402 ) ;
#25622 = EDGE_CURVE ( 'NONE', #3747, #17603, #27863, .T. ) ;
#25623 = AXIS2_PLACEMENT_3D ( 'NONE', #8295, #348, #12623 ) ;
#25624 = VERTEX_POINT ( 'NONE', #16967 ) ;
#25625 = ORIENTED_EDGE ( 'NONE', *, *, #13050, .T. ) ;
#25626 = CARTESIAN_POINT ( 'NONE',  ( 158.0000000000007958, 128.7164997297464595, 45.00000000000000000 ) ) ;
#25627 = VECTOR ( 'NONE', #24435, 999.9999999999998863 ) ;
#25628 = EDGE_CURVE ( 'NONE', #5518, #25999, #1868, .T. ) ;
#25629 = CARTESIAN_POINT ( 'NONE',  ( 157.4999999999998579, 196.1751874286831026, 45.00000000000000000 ) ) ;
#25630 = DIRECTION ( 'NONE',  ( 0.8916010070293783896, -0.4528218681382319422, 0.000000000000000000 ) ) ;
#25631 = DIRECTION ( 'NONE',  ( 0.000000000000000000, -1.000000000000000000, 0.000000000000000000 ) ) ;
#25632 = CARTESIAN_POINT ( 'NONE',  ( 157.4999999999998579, 105.8916871584295478, 45.00000000000000000 ) ) ;
#25633 = DIRECTION ( 'NONE',  ( -1.850371707708594316E-16, 1.000000000000000000, -0.000000000000000000 ) ) ;
#25634 = CARTESIAN_POINT ( 'NONE',  ( -230.0306293838648912, 64.31401865984727806, -16.82661551914406317 ) ) ;
#25635 = PRODUCT_DEFINITION ( 'UNKNOWN', '', #25780, #11192 ) ;
#25636 = AXIS2_PLACEMENT_3D ( 'NONE', #2177, #17414, #326 ) ;
#25637 = LINE ( 'NONE', #10143, #27587 ) ;
#25638 = CARTESIAN_POINT ( 'NONE',  ( 158.0000000000005400, 158.3031248123239436, 45.00000000000000000 ) ) ;
#25639 = LINE ( 'NONE', #28209, #4758 ) ;
#25640 = EDGE_LOOP ( 'NONE', ( #8603, #6668 ) ) ;
#25641 = CARTESIAN_POINT ( 'NONE',  ( 0.000000000000000000, 1.249999999999999556, -6.997769477110050929 ) ) ;
#25642 = AXIS2_PLACEMENT_3D ( 'NONE', #3945, #6246, #6106 ) ;
#25643 = CARTESIAN_POINT ( 'NONE',  ( 1.633516369018862102, -1.250000000000000444, 7.514731128045609942 ) ) ;
#25644 = DIRECTION ( 'NONE',  ( 1.000000000000000000, 0.000000000000000000, 0.000000000000000000 ) ) ;
#25645 =( LENGTH_UNIT ( ) NAMED_UNIT ( * ) SI_UNIT ( .MILLI., .METRE. ) );
#25646 = CARTESIAN_POINT ( 'NONE',  ( -25.39999999999996305, 6.123233995736766282E-16, -5.000000000000000000 ) ) ;
#25647 = VERTEX_POINT ( 'NONE', #13961 ) ;
#25648 = AXIS2_PLACEMENT_3D ( 'NONE', #11807, #20547, #872 ) ;
#25649 = CARTESIAN_POINT ( 'NONE',  ( 157.9999999999996589, 278.6811251726610976, 45.00000000000000000 ) ) ;
#25650 = ORIENTED_EDGE ( 'NONE', *, *, #22501, .T. ) ;
#25651 = DIRECTION ( 'NONE',  ( 1.321694076934710155E-16, -1.000000000000000000, 0.000000000000000000 ) ) ;
#25652 = ORIENTED_EDGE ( 'NONE', *, *, #16592, .T. ) ;
#25653 = EDGE_LOOP ( 'NONE', ( #25439, #16099, #15214, #25486 ) ) ;
#25654 = CARTESIAN_POINT ( 'NONE',  ( -43.02437977270768243, 129.7200458115292747, 16.81627168235289460 ) ) ;
#25655 = EDGE_CURVE ( 'NONE', #16800, #13530, #9932, .T. ) ;
#25656 = EDGE_CURVE ( 'NONE', #17953, #7888, #26867, .T. ) ;
#25657 = VECTOR ( 'NONE', #6837, 1000.000000000000000 ) ;
#25658 = VECTOR ( 'NONE', #12685, 1000.000000000000000 ) ;
#25659 = ORIENTED_EDGE ( 'NONE', *, *, #7453, .F. ) ;
#25660 = ORIENTED_EDGE ( 'NONE', *, *, #757, .F. ) ;
#25661 = FACE_OUTER_BOUND ( 'NONE', #6427, .T. ) ;
#25662 = CARTESIAN_POINT ( 'NONE',  ( -190.0000000000000284, 59.99999999999995026, 80.00000000000001421 ) ) ;
#25663 = DIRECTION ( 'NONE',  ( 0.000000000000000000, 0.000000000000000000, -1.000000000000000000 ) ) ;
#25664 = CIRCLE ( 'NONE', #5463, 70.83858790703926900 ) ;
#25665 = CARTESIAN_POINT ( 'NONE',  ( -148.0316173832768527, 125.5119630376401432, -18.70358149194362340 ) ) ;
#25666 = CIRCLE ( 'NONE', #8223, 5.999999999999977796 ) ;
#25667 = CARTESIAN_POINT ( 'NONE',  ( -270.7973404499905428, -170.2932079548401987, -93.47773194822650566 ) ) ;
#25668 = CARTESIAN_POINT ( 'NONE',  ( 156.9574749595459195, 226.9187638636467739, 45.00000000000000000 ) ) ;
#25669 = LINE ( 'NONE', #5851, #8494 ) ;
#25670 = CARTESIAN_POINT ( 'NONE',  ( -218.1021218244185604, 87.79535473091540609, -19.36533790319589698 ) ) ;
#25671 = EDGE_CURVE ( 'NONE', #13771, #1877, #11518, .T. ) ;
#25672 = EDGE_CURVE ( 'NONE', #24608, #11100, #2439, .T. ) ;
#25673 = CARTESIAN_POINT ( 'NONE',  ( 158.0000000000011653, 95.60624962464788723, 45.00000000000000000 ) ) ;
#25674 = CARTESIAN_POINT ( 'NONE',  ( 157.9999999999996589, 276.6811251726610976, 45.00000000000000000 ) ) ;
#25675 = LINE ( 'NONE', #6424, #70 ) ;
#25676 = DIRECTION ( 'NONE',  ( -0.000000000000000000, 0.000000000000000000, -1.000000000000000000 ) ) ;
#25677 = LINE ( 'NONE', #12766, #25384 ) ;
#25678 = EDGE_LOOP ( 'NONE', ( #2073, #16886, #18809, #16240 ) ) ;
#25679 = VECTOR ( 'NONE', #1367, 1000.000000000000114 ) ;
#25680 = CARTESIAN_POINT ( 'NONE',  ( 67.86343429515802939, -22.14858123305036486, 45.00000000000000000 ) ) ;
#25681 = CARTESIAN_POINT ( 'NONE',  ( -277.2150368962633706, -170.0000000000001137, -110.0000000000000284 ) ) ;
#25682 = DIRECTION ( 'NONE',  ( 0.4528218681380503097, -0.8916010070294707601, 0.000000000000000000 ) ) ;
#25684 = ORIENTED_EDGE ( 'NONE', *, *, #26446, .T. ) ;
#25683 = ORIENTED_EDGE ( 'NONE', *, *, #13685, .F. ) ;
#25685 = EDGE_CURVE ( 'NONE', #4413, #3398, #17816, .T. ) ;
#25686 = CIRCLE ( 'NONE', #7789, 1.999999999999997335 ) ;
#25687 = ADVANCED_FACE ( 'NONE', ( #6900 ), #15064, .T. ) ;
#25688 = CARTESIAN_POINT ( 'NONE',  ( 96.03789414441068573, 240.4739163874471330, -19.46186845665527443 ) ) ;
#25689 = VERTEX_POINT ( 'NONE', #27663 ) ;
#25690 = ORIENTED_EDGE ( 'NONE', *, *, #11146, .T. ) ;
#25691 = ORIENTED_EDGE ( 'NONE', *, *, #5004, .F. ) ;
#25692 = EDGE_LOOP ( 'NONE', ( #7694, #3804, #7262, #2433 ) ) ;
#25693 = EDGE_CURVE ( 'NONE', #6606, #7851, #27804, .T. ) ;
#25694 = VERTEX_POINT ( 'NONE', #21489 ) ;
#25695 = ORIENTED_EDGE ( 'NONE', *, *, #14168, .F. ) ;
#25696 = DIRECTION ( 'NONE',  ( -0.8916010070293383105, -0.4528218681383106015, 0.000000000000000000 ) ) ;
#25697 = VECTOR ( 'NONE', #12587, 1000.000000000000000 ) ;
#25698 = CARTESIAN_POINT ( 'NONE',  ( -141.6428522700808230, 22.24192588826928585, 83.00000000000001421 ) ) ;
#25699 = PLANE ( 'NONE',  #27670 ) ;
#25700 = VECTOR ( 'NONE', #24261, 1000.000000000000000 ) ;
#25701 = CARTESIAN_POINT ( 'NONE',  ( 158.0000000000000000, 208.4606249624626457, 45.00000000000000000 ) ) ;
#25702 = EDGE_CURVE ( 'NONE', #8924, #4742, #1531, .T. ) ;
#25703 = LINE ( 'NONE', #25424, #23155 ) ;
#25704 = FACE_OUTER_BOUND ( 'NONE', #13096, .T. ) ;
#25705 = CARTESIAN_POINT ( 'NONE',  ( -194.4086842179900714, 63.14614340836796913, -41.97977085781615614 ) ) ;
#25706 = CARTESIAN_POINT ( 'NONE',  ( 112.1359432235843059, 200.5768536076146233, -142.3325995572699298 ) ) ;
#25707 = CARTESIAN_POINT ( 'NONE',  ( 184.9999999999999432, -327.2004514666934369, -84.99999999999997158 ) ) ;
#25708 = DIRECTION ( 'NONE',  ( 0.000000000000000000, 0.000000000000000000, 1.000000000000000000 ) ) ;
#25709 = CARTESIAN_POINT ( 'NONE',  ( 158.0000000000000853, 200.9369999399436892, 45.00000000000000000 ) ) ;
#25710 = ORIENTED_EDGE ( 'NONE', *, *, #12060, .T. ) ;
#25711 = CARTESIAN_POINT ( 'NONE',  ( 115.9304285313508700, 231.9550723406498776, -99.14012769162694383 ) ) ;
#25712 = VECTOR ( 'NONE', #27782, 1000.000000000000000 ) ;
#25713 = DIRECTION ( 'NONE',  ( 1.000000000000000000, 0.000000000000000000, 0.000000000000000000 ) ) ;
#25714 = ORIENTED_EDGE ( 'NONE', *, *, #14198, .T. ) ;
#25715 = ORIENTED_EDGE ( 'NONE', *, *, #11615, .T. ) ;
#25716 = EDGE_CURVE ( 'NONE', #1393, #20275, #13618, .T. ) ;
#25718 = EDGE_CURVE ( 'NONE', #3367, #28150, #23509, .T. ) ;
#25717 = ORIENTED_EDGE ( 'NONE', *, *, #5673, .F. ) ;
#25719 = VECTOR ( 'NONE', #16060, 1000.000000000000000 ) ;
#25720 = PLANE ( 'NONE',  #21666 ) ;
#25721 = DIRECTION ( 'NONE',  ( 0.8916010070293515222, 0.4528218681382848443, 0.000000000000000000 ) ) ;
#25722 = ORIENTED_EDGE ( 'NONE', *, *, #6195, .T. ) ;
#25723 = ADVANCED_FACE ( 'NONE', ( #1671 ), #10439, .F. ) ;
#25724 = ORIENTED_EDGE ( 'NONE', *, *, #6008, .F. ) ;
#25725 = LINE ( 'NONE', #10228, #25104 ) ;
#25726 = CARTESIAN_POINT ( 'NONE',  ( 106.6902265666634122, 244.3124981716793513, 31.28096500751039599 ) ) ;
#25727 = DIRECTION ( 'NONE',  ( 1.000000000000000000, 0.000000000000000000, -2.220446049250266932E-15 ) ) ;
#25728 = ORIENTED_EDGE ( 'NONE', *, *, #21939, .F. ) ;
#25729 = DIRECTION ( 'NONE',  ( 1.000000000000000000, 0.000000000000000000, 0.000000000000000000 ) ) ;
#25730 = ORIENTED_EDGE ( 'NONE', *, *, #26305, .T. ) ;
#25731 = LINE ( 'NONE', #28164, #1522 ) ;
#25732 = VECTOR ( 'NONE', #4184, 1000.000000000000000 ) ;
#25733 = DIRECTION ( 'NONE',  ( -0.8916010070297446521, -0.4528218681375106858, 0.000000000000000000 ) ) ;
#25734 = LINE ( 'NONE', #6203, #12807 ) ;
#25735 = DIRECTION ( 'NONE',  ( 0.000000000000000000, 0.000000000000000000, -1.000000000000000000 ) ) ;
#25736 = AXIS2_PLACEMENT_3D ( 'NONE', #5888, #13088, #15091 ) ;
#25737 = CARTESIAN_POINT ( 'NONE',  ( 161.3687566780243685, 205.6878092301651009, -150.9609010065648818 ) ) ;
#25738 = VERTEX_POINT ( 'NONE', #8284 ) ;
#25739 = CARTESIAN_POINT ( 'NONE',  ( 119.9999999999999147, 140.0000000000000000, 100.0000000000000142 ) ) ;
#25740 = CARTESIAN_POINT ( 'NONE',  ( 367.4999999999996021, -5.589247009368139452, -75.00000000000001421 ) ) ;
#25741 = FACE_BOUND ( 'NONE', #16491, .T. ) ;
#25742 = CARTESIAN_POINT ( 'NONE',  ( 157.9999999999997158, 263.6338751276190351, 45.00000000000000000 ) ) ;
#25743 = ORIENTED_EDGE ( 'NONE', *, *, #18917, .F. ) ;
#25744 = CARTESIAN_POINT ( 'NONE',  ( 116.2340178909017396, 232.4263996303828606, 99.27034901580076109 ) ) ;
#25745 = FACE_OUTER_BOUND ( 'NONE', #18585, .T. ) ;
#25746 = PLANE ( 'NONE',  #11035 ) ;
#25747 = CARTESIAN_POINT ( 'NONE',  ( -225.7485474213321481, 89.51658778958633889, 13.99034047932378755 ) ) ;
#25748 = VERTEX_POINT ( 'NONE', #17185 ) ;
#25749 = CARTESIAN_POINT ( 'NONE',  ( 147.3660254037842492, 239.4185842870417673, -45.00000000000000000 ) ) ;
#25750 = EDGE_CURVE ( 'NONE', #17968, #25123, #25942, .T. ) ;
#25751 = ORIENTED_EDGE ( 'NONE', *, *, #2369, .T. ) ;
#25752 = EDGE_CURVE ( 'NONE', #16142, #19893, #11801, .T. ) ;
#25753 = EDGE_CURVE ( 'NONE', #11803, #1940, #17606, .T. ) ;
#25754 = VECTOR ( 'NONE', #14178, 1000.000000000000000 ) ;
#25755 = FACE_OUTER_BOUND ( 'NONE', #20252, .T. ) ;
#25756 = ADVANCED_FACE ( 'NONE', ( #2508, #17318 ), #6689, .F. ) ;
#25757 = PLANE ( 'NONE',  #18629 ) ;
#25758 = ORIENTED_EDGE ( 'NONE', *, *, #24958, .F. ) ;
#25759 = VECTOR ( 'NONE', #18697, 1000.000000000000000 ) ;
#25760 = AXIS2_PLACEMENT_3D ( 'NONE', #20741, #7545, #21164 ) ;
#25761 = ORIENTED_EDGE ( 'NONE', *, *, #24894, .T. ) ;
#25762 = CARTESIAN_POINT ( 'NONE',  ( 158.0000000000013074, 83.06687458711267880, 45.00000000000000000 ) ) ;
#25763 = ORIENTED_EDGE ( 'NONE', *, *, #14271, .F. ) ;
#25764 = AXIS2_PLACEMENT_3D ( 'NONE', #10892, #20213, #24379 ) ;
#25765 = ORIENTED_EDGE ( 'NONE', *, *, #3719, .F. ) ;
#25766 = EDGE_LOOP ( 'NONE', ( #24253, #24049, #1201, #9135, #3245, #16133 ) ) ;
#25767 = DIRECTION ( 'NONE',  ( 0.000000000000000000, 0.000000000000000000, -1.000000000000000000 ) ) ;
#25768 = DIRECTION ( 'NONE',  ( 0.000000000000000000, 0.000000000000000000, -1.000000000000000000 ) ) ;
#25769 = CARTESIAN_POINT ( 'NONE',  ( 0.3651377029009472142, 1.249999999999999556, 7.402212548643259282 ) ) ;
#25770 = DIRECTION ( 'NONE',  ( 0.000000000000000000, 0.000000000000000000, -1.000000000000000000 ) ) ;
#25771 = LINE ( 'NONE', #23766, #7827 ) ;
#25772 = DIRECTION ( 'NONE',  ( 0.000000000000000000, 0.000000000000000000, -1.000000000000000000 ) ) ;
#25773 = CARTESIAN_POINT ( 'NONE',  ( -236.8177751472017007, 82.33896643611701904, -15.00000000000000178 ) ) ;
#25774 = ORIENTED_EDGE ( 'NONE', *, *, #3674, .T. ) ;
#25775 = AXIS2_PLACEMENT_3D ( 'NONE', #4499, #6671, #209 ) ;
#25776 = PLANE ( 'NONE',  #12247 ) ;
#25777 = CARTESIAN_POINT ( 'NONE',  ( 155.2453482286826727, 220.0000000000000284, -189.9999999999999716 ) ) ;
#25778 = CARTESIAN_POINT ( 'NONE',  ( -175.0000000000000000, -120.0000000000001847, -69.99999999999998579 ) ) ;
#25779 = CARTESIAN_POINT ( 'NONE',  ( 112.5712424644275131, 222.0554180856713060, -96.69730840357117074 ) ) ;
#25780 = PRODUCT_DEFINITION_FORMATION_WITH_SPECIFIED_SOURCE ( 'ANY', '', #1547, .NOT_KNOWN. ) ;
#25781 = VERTEX_POINT ( 'NONE', #4104 ) ;
#25782 = CARTESIAN_POINT ( 'NONE',  ( 0.1708624500919104228, 1.249999999999999556, -7.345492880323159390 ) ) ;
#25783 = EDGE_CURVE ( 'NONE', #170, #17429, #21634, .T. ) ;
#25784 = VECTOR ( 'NONE', #12601, 999.9999999999998863 ) ;
#25785 = EDGE_CURVE ( 'NONE', #25171, #6014, #10729, .T. ) ;
#25786 = DIRECTION ( 'NONE',  ( 0.8916010070294395629, -0.4528218681381114274, 0.000000000000000000 ) ) ;
#25787 = DIRECTION ( 'NONE',  ( 1.000000000000000000, 0.000000000000000000, 0.000000000000000000 ) ) ;
#25788 = CARTESIAN_POINT ( 'NONE',  ( -63.57415822541634043, 0.000000000000000000, 95.00000000000000000 ) ) ;
#25789 = PLANE ( 'NONE',  #13231 ) ;
#25790 = FACE_OUTER_BOUND ( 'NONE', #6550, .T. ) ;
#25791 = ORIENTED_EDGE ( 'NONE', *, *, #5590, .F. ) ;
#25792 = ADVANCED_FACE ( 'NONE', ( #12889 ), #4387, .F. ) ;
#25793 = SPHERICAL_SURFACE ( 'NONE', #28114, 35.18636678425505693 ) ;
#25794 = ORIENTED_EDGE ( 'NONE', *, *, #3861, .T. ) ;
#25795 = EDGE_CURVE ( 'NONE', #18838, #9458, #10867, .T. ) ;
#25796 = LINE ( 'NONE', #23648, #22278 ) ;
#25797 = EDGE_LOOP ( 'NONE', ( #2511, #17765, #19898, #12528 ) ) ;
#25798 = AXIS2_PLACEMENT_3D ( 'NONE', #14908, #1676, #28092 ) ;
#25799 = EDGE_LOOP ( 'NONE', ( #21629, #6198, #9965, #8638 ) ) ;
#25800 = CARTESIAN_POINT ( 'NONE',  ( -75.20817585874782196, 134.4830317599007685, 15.51105434715999465 ) ) ;
#25801 = VECTOR ( 'NONE', #14813, 1000.000000000000114 ) ;
#25802 = ORIENTED_EDGE ( 'NONE', *, *, #1564, .F. ) ;
#25803 = ORIENTED_EDGE ( 'NONE', *, *, #10935, .T. ) ;
#25804 = CARTESIAN_POINT ( 'NONE',  ( 158.0000000000005969, 148.7794997898028271, 45.00000000000000000 ) ) ;
#25805 = CARTESIAN_POINT ( 'NONE',  ( -134.4422573331441697, 128.5907357665044799, -17.24671386403461071 ) ) ;
#25806 = CARTESIAN_POINT ( 'NONE',  ( -211.3305068427980586, -219.3267326664164614, 91.92140052019108509 ) ) ;
#25807 = VECTOR ( 'NONE', #19965, 1000.000000000000000 ) ;
#25808 = CARTESIAN_POINT ( 'NONE',  ( -112.7304692548805605, 133.0259997015394333, -15.80934902741073067 ) ) ;
#25809 = FACE_OUTER_BOUND ( 'NONE', #25678, .T. ) ;
#25810 = CARTESIAN_POINT ( 'NONE',  ( -160.0000000000000284, 139.9999999999999716, 45.00000000000000000 ) ) ;
#25811 = CARTESIAN_POINT ( 'NONE',  ( -261.1919288306253293, -171.9377729149742038, 95.00000000000001421 ) ) ;
#25812 = CARTESIAN_POINT ( 'NONE',  ( -220.0227340339567661, 87.95399931298469198, -18.35314071734302388 ) ) ;
#25813 = CARTESIAN_POINT ( 'NONE',  ( -146.6428522700808230, 17.24192588826928585, 83.00000000000001421 ) ) ;
#25814 = CARTESIAN_POINT ( 'NONE',  ( 140.5127944162910865, 243.3752990424897575, -45.00000000000000000 ) ) ;
#25815 = EDGE_CURVE ( 'NONE', #18495, #14427, #14070, .T. ) ;
#25816 = LINE ( 'NONE', #19074, #19323 ) ;
#25817 = DIRECTION ( 'NONE',  ( 0.000000000000000000, 0.000000000000000000, -1.000000000000000000 ) ) ;
#25818 = DIRECTION ( 'NONE',  ( 0.000000000000000000, 1.000000000000000000, 0.000000000000000000 ) ) ;
#25819 = ORIENTED_EDGE ( 'NONE', *, *, #25877, .F. ) ;
#25820 = VECTOR ( 'NONE', #20010, 1000.000000000000000 ) ;
#25821 = EDGE_CURVE ( 'NONE', #15637, #9868, #8707, .T. ) ;
#25822 = CIRCLE ( 'NONE', #10673, 17.93072811908088937 ) ;
#25823 = DIRECTION ( 'NONE',  ( -0.8916010070298868717, -0.4528218681372309651, 0.000000000000000000 ) ) ;
#25824 = DIRECTION ( 'NONE',  ( 0.000000000000000000, 0.000000000000000000, -1.000000000000000000 ) ) ;
#25825 = DIRECTION ( 'NONE',  ( -0.000000000000000000, -0.000000000000000000, 1.000000000000000000 ) ) ;
#25826 = CIRCLE ( 'NONE', #28089, 30.00000000000000000 ) ;
#25828 = ORIENTED_EDGE ( 'NONE', *, *, #8505, .T. ) ;
#25827 = ORIENTED_EDGE ( 'NONE', *, *, #6916, .F. ) ;
#25829 = VECTOR ( 'NONE', #5834, 1000.000000000000000 ) ;
#25830 = CARTESIAN_POINT ( 'NONE',  ( 95.18208312637753465, 240.6790578601106745, -9.159889466453034146 ) ) ;
#25831 = ORIENTED_EDGE ( 'NONE', *, *, #14468, .F. ) ;
#25832 = ORIENTED_EDGE ( 'NONE', *, *, #10850, .T. ) ;
#25833 = ORIENTED_EDGE ( 'NONE', *, *, #19928, .T. ) ;
#25834 = EDGE_CURVE ( 'NONE', #19162, #23817, #4248, .T. ) ;
#25835 = EDGE_LOOP ( 'NONE', ( #1338, #14475, #2512, #24171 ) ) ;
#25836 = ORIENTED_EDGE ( 'NONE', *, *, #25278, .F. ) ;
#25837 = ORIENTED_EDGE ( 'NONE', *, *, #19275, .T. ) ;
#25838 = DIRECTION ( 'NONE',  ( 1.000000000000000000, 0.000000000000000000, 0.000000000000000000 ) ) ;
#25839 = AXIS2_PLACEMENT_3D ( 'NONE', #22479, #71, #24489 ) ;
#25840 = FACE_OUTER_BOUND ( 'NONE', #20079, .T. ) ;
#25841 = VECTOR ( 'NONE', #7840, 1000.000000000000000 ) ;
#25842 = CARTESIAN_POINT ( 'NONE',  ( 109.9999999999999005, 259.7997850037947956, -44.82660872220826320 ) ) ;
#25843 = EDGE_CURVE ( 'NONE', #21211, #26462, #21918, .T. ) ;
#25844 = FACE_OUTER_BOUND ( 'NONE', #13288, .T. ) ;
#25845 = DIRECTION ( 'NONE',  ( 0.000000000000000000, 1.000000000000000000, 0.000000000000000000 ) ) ;
#25846 = CARTESIAN_POINT ( 'NONE',  ( 158.0000000000009379, 118.1771246922112653, -45.00000000000000000 ) ) ;
#25847 = DIRECTION ( 'NONE',  ( 1.000000000000000000, 0.000000000000000000, 0.000000000000000000 ) ) ;
#25848 = EDGE_CURVE ( 'NONE', #20650, #23124, #20009, .T. ) ;
#25849 = CARTESIAN_POINT ( 'NONE',  ( -42.65532241761712839, 131.0044336801082352, 16.34779397420836844 ) ) ;
#25850 = DIRECTION ( 'NONE',  ( 0.000000000000000000, -1.000000000000000000, 0.000000000000000000 ) ) ;
#25851 = CARTESIAN_POINT ( 'NONE',  ( -200.0000000000000284, -120.0000000000001847, 25.00000000000001776 ) ) ;
#25852 = CARTESIAN_POINT ( 'NONE',  ( -68.57415822541635464, -23.01420295945612082, 100.0000000000000000 ) ) ;
#25853 = ORIENTED_EDGE ( 'NONE', *, *, #21678, .F. ) ;
#25854 = CIRCLE ( 'NONE', #17146, 16.46313063346208239 ) ;
#25855 = CARTESIAN_POINT ( 'NONE',  ( -174.8584600856924283, 112.6472680211073936, 28.91287214637171132 ) ) ;
#25856 = PRODUCT_DEFINITION_SHAPE ( 'NONE', 'NONE',  #3316 ) ;
#25857 = DIRECTION ( 'NONE',  ( -0.000000000000000000, -0.000000000000000000, -1.000000000000000000 ) ) ;
#25858 = ORIENTED_EDGE ( 'NONE', *, *, #9420, .F. ) ;
#25859 = PRODUCT_CONTEXT ( 'NONE', #4132, 'mechanical' ) ;
#25860 = VECTOR ( 'NONE', #6247, 1000.000000000000000 ) ;
#25861 = ORIENTED_EDGE ( 'NONE', *, *, #15371, .T. ) ;
#25862 = EDGE_LOOP ( 'NONE', ( #6905, #3769, #17316, #26329, #1000, #6000 ) ) ;
#25863 = EDGE_CURVE ( 'NONE', #23690, #19503, #8570, .T. ) ;
#25864 = EDGE_CURVE ( 'NONE', #5196, #19742, #9134, .T. ) ;
#25865 = CARTESIAN_POINT ( 'NONE',  ( 119.7545560453059892, 132.4900181921427702, 100.0000000000000142 ) ) ;
#25866 = LINE ( 'NONE', #8205, #26423 ) ;
#25867 = ORIENTED_EDGE ( 'NONE', *, *, #8389, .F. ) ;
#25868 = VERTEX_POINT ( 'NONE', #26361 ) ;
#25869 = CARTESIAN_POINT ( 'NONE',  ( 107.3061218092339715, 127.3934823308176760, -87.81249999970602005 ) ) ;
#25870 = CARTESIAN_POINT ( 'NONE',  ( 100.0424040729205188, 235.0879316926391596, 22.67296783064056243 ) ) ;
#25871 = CARTESIAN_POINT ( 'NONE',  ( -180.0000000000000284, 59.99999999999994316, -70.00000000000001421 ) ) ;
#25872 = ORIENTED_EDGE ( 'NONE', *, *, #7432, .F. ) ;
#25873 = CARTESIAN_POINT ( 'NONE',  ( -207.2993993385316855, 89.56313076513357885, 27.29723889156834105 ) ) ;
#25874 = EDGE_LOOP ( 'NONE', ( #8322, #3322, #9237, #7080 ) ) ;
#25875 = CIRCLE ( 'NONE', #15819, 2.000000000000004885 ) ;
#25876 = CARTESIAN_POINT ( 'NONE',  ( 157.4999999999998579, 128.4625622259929401, -45.00000000000000000 ) ) ;
#25877 = EDGE_CURVE ( 'NONE', #19152, #26356, #15471, .T. ) ;
#25878 = CARTESIAN_POINT ( 'NONE',  ( -63.57415822541634043, 75.97823757117562593, 95.00000000000000000 ) ) ;
#25879 = VECTOR ( 'NONE', #14109, 1000.000000000000000 ) ;
#25880 = FACE_OUTER_BOUND ( 'NONE', #13720, .T. ) ;
#25881 = EDGE_CURVE ( 'NONE', #372, #12774, #4523, .T. ) ;
#25882 = ADVANCED_FACE ( 'NONE', ( #22206 ), #26494, .F. ) ;
#25883 = DIRECTION ( 'NONE',  ( 0.4528218681382319422, 0.8916010070293783896, -0.000000000000000000 ) ) ;
#25884 = ORIENTED_EDGE ( 'NONE', *, *, #6137, .F. ) ;
#25885 = DIRECTION ( 'NONE',  ( 0.000000000000000000, 0.000000000000000000, 1.000000000000000000 ) ) ;
#25886 = ADVANCED_FACE ( 'NONE', ( #19483 ), #24351, .F. ) ;
#25887 = CARTESIAN_POINT ( 'NONE',  ( -270.1025481742786951, -91.18033988749901653, -11.42311362948588105 ) ) ;
#25888 = PLANE ( 'NONE',  #17976 ) ;
#25889 = PLANE ( 'NONE',  #13979 ) ;
#25890 = VERTEX_POINT ( 'NONE', #1944 ) ;
#25891 = FACE_OUTER_BOUND ( 'NONE', #12641, .T. ) ;
#25892 = CARTESIAN_POINT ( 'NONE',  ( -192.4016700810780094, 101.6532444370910468, 31.99634417553368948 ) ) ;
#25893 = CARTESIAN_POINT ( 'NONE',  ( -260.0000000000001137, -157.0000000000000284, -89.99999999999985789 ) ) ;
#25894 = DIRECTION ( 'NONE',  ( 0.000000000000000000, 0.000000000000000000, 1.000000000000000000 ) ) ;
#25895 = EDGE_LOOP ( 'NONE', ( #22181, #6643, #24344, #1281 ) ) ;
#25896 = DIRECTION ( 'NONE',  ( 1.321694076934710155E-16, -1.000000000000000000, 0.000000000000000000 ) ) ;
#25897 = VERTEX_POINT ( 'NONE', #7557 ) ;
#25898 = AXIS2_PLACEMENT_3D ( 'NONE', #12973, #10805, #23730 ) ;
#25899 = CARTESIAN_POINT ( 'NONE',  ( -151.0494637935773881, 123.3493803929174391, 20.02198554298006528 ) ) ;
#25900 = CARTESIAN_POINT ( 'NONE',  ( -184.1540942457759229, 107.3771663064187152, -31.09098462597617996 ) ) ;
#25901 = VERTEX_POINT ( 'NONE', #11733 ) ;
#25902 = EDGE_CURVE ( 'NONE', #27860, #25890, #23692, .T. ) ;
#25903 = ORIENTED_EDGE ( 'NONE', *, *, #16572, .F. ) ;
#25904 = CARTESIAN_POINT ( 'NONE',  ( 157.4999999999996589, 273.9193126614005678, 45.00000000000000000 ) ) ;
#25905 = ORIENTED_EDGE ( 'NONE', *, *, #12455, .T. ) ;
#25906 = ORIENTED_EDGE ( 'NONE', *, *, #400, .F. ) ;
#25907 = EDGE_LOOP ( 'NONE', ( #9948, #14302, #19567, #14193 ) ) ;
#25908 = CARTESIAN_POINT ( 'NONE',  ( 158.0000000000000853, 198.9369999399436892, -45.00000000000000000 ) ) ;
#25909 = FACE_OUTER_BOUND ( 'NONE', #26802, .T. ) ;
#25910 = VECTOR ( 'NONE', #944, 1000.000000000000000 ) ;
#25911 = DIRECTION ( 'NONE',  ( -0.000000000000000000, 0.000000000000000000, -1.000000000000000000 ) ) ;
#25912 = DIRECTION ( 'NONE',  ( -0.000000000000000000, -0.000000000000000000, -1.000000000000000000 ) ) ;
#25913 = AXIS2_PLACEMENT_3D ( 'NONE', #8043, #23700, #18817 ) ;
#25914 = EDGE_CURVE ( 'NONE', #19932, #17959, #11445, .T. ) ;
#25915 = EDGE_CURVE ( 'NONE', #15321, #4251, #25996, .T. ) ;
#25916 = LINE ( 'NONE', #6099, #25697 ) ;
#25917 = LINE ( 'NONE', #14881, #25492 ) ;
#25918 = CARTESIAN_POINT ( 'NONE',  ( -230.6867234551526167, 75.40543009380724016, -15.98884730489883665 ) ) ;
#25919 = ORIENTED_EDGE ( 'NONE', *, *, #13358, .T. ) ;
#25920 = CARTESIAN_POINT ( 'NONE',  ( 46.79174272583949090, 194.0572550123460474, -15.00000000000000000 ) ) ;
#25921 = CIRCLE ( 'NONE', #13557, 5.000000000000004441 ) ;
#25922 = LINE ( 'NONE', #17021, #17955 ) ;
#25923 = DIRECTION ( 'NONE',  ( -0.000000000000000000, -1.000000000000000000, -0.000000000000000000 ) ) ;
#25924 = CARTESIAN_POINT ( 'NONE',  ( 158.0000000000006537, 143.2558747672816821, -45.00000000000000000 ) ) ;
#25925 = ORIENTED_EDGE ( 'NONE', *, *, #924, .F. ) ;
#25926 = CARTESIAN_POINT ( 'NONE',  ( 12.78000883847031588, 237.8887863075477469, 45.00000000000000000 ) ) ;
#25927 = DIRECTION ( 'NONE',  ( 0.4528218681379903021, -0.8916010070295011802, 0.000000000000000000 ) ) ;
#25928 = DIRECTION ( 'NONE',  ( 0.000000000000000000, 0.000000000000000000, -1.000000000000000000 ) ) ;
#25929 = DIRECTION ( 'NONE',  ( 0.4528218681381501742, -0.8916010070294199119, 0.000000000000000000 ) ) ;
#25930 = CARTESIAN_POINT ( 'NONE',  ( 232.4999999999996305, 83.06687458711267880, -42.88984227207694033 ) ) ;
#25931 = FACE_OUTER_BOUND ( 'NONE', #5731, .T. ) ;
#25932 = ORIENTED_EDGE ( 'NONE', *, *, #6713, .T. ) ;
#25933 = DIRECTION ( 'NONE',  ( 0.000000000000000000, 0.000000000000000000, -1.000000000000000000 ) ) ;
#25934 = ORIENTED_EDGE ( 'NONE', *, *, #22908, .F. ) ;
#25935 = ADVANCED_FACE ( 'NONE', ( #13744 ), #9428, .F. ) ;
#25936 = CARTESIAN_POINT ( 'NONE',  ( 158.0000000000015916, 55.48024950453520177, -45.00000000000000000 ) ) ;
#25937 = ORIENTED_EDGE ( 'NONE', *, *, #24249, .F. ) ;
#25938 = VECTOR ( 'NONE', #8541, 1000.000000000000000 ) ;
#25939 = VECTOR ( 'NONE', #12865, 1000.000000000000000 ) ;
#25940 = VECTOR ( 'NONE', #3840, 1000.000000000000000 ) ;
#25941 = ORIENTED_EDGE ( 'NONE', *, *, #27975, .T. ) ;
#25942 = LINE ( 'NONE', #865, #750 ) ;
#25943 = ORIENTED_EDGE ( 'NONE', *, *, #19925, .T. ) ;
#25944 = EDGE_CURVE ( 'NONE', #695, #12922, #3079, .T. ) ;
#25945 = ORIENTED_EDGE ( 'NONE', *, *, #25013, .T. ) ;
#25946 = VECTOR ( 'NONE', #10215, 1000.000000000000227 ) ;
#25947 = ORIENTED_EDGE ( 'NONE', *, *, #28012, .T. ) ;
#25948 = LINE ( 'NONE', #6267, #5393 ) ;
#25949 = CARTESIAN_POINT ( 'NONE',  ( -62.68650544878820341, 133.3634780166508165, -15.73273055292821354 ) ) ;
#25950 = DIRECTION ( 'NONE',  ( -0.000000000000000000, -0.000000000000000000, -1.000000000000000000 ) ) ;
#25951 = CARTESIAN_POINT ( 'NONE',  ( -156.3896018538470116, 122.2161512765613480, -19.69795454272433233 ) ) ;
#25952 = EDGE_CURVE ( 'NONE', #27147, #27590, #23242, .T. ) ;
#25953 = ADVANCED_FACE ( 'NONE', ( #7122 ), #518, .F. ) ;
#25954 = CARTESIAN_POINT ( 'NONE',  ( -263.9486459716463855, -171.3073464501530907, -94.90637380402192491 ) ) ;
#25955 = DIRECTION ( 'NONE',  ( -0.8916010070299172918, -0.4528218681371710685, 0.000000000000000000 ) ) ;
#25956 = CARTESIAN_POINT ( 'NONE',  ( -228.4262338387342197, 88.49915910525061236, -15.54344599199708910 ) ) ;
#25957 = EDGE_CURVE ( 'NONE', #5675, #1568, #14162, .T. ) ;
#25958 = CARTESIAN_POINT ( 'NONE',  ( 129.0397224731839287, 249.4020613294620148, -144.2074248490017396 ) ) ;
#25959 = CIRCLE ( 'NONE', #15412, 18.46313063346208239 ) ;
#25960 = DIRECTION ( 'NONE',  ( -0.7071067811865474617, -0.7071067811865474617, 0.000000000000000000 ) ) ;
#25961 = DIRECTION ( 'NONE',  ( 1.000000000000000000, -0.000000000000000000, -0.000000000000000000 ) ) ;
#25962 = PLANE ( 'NONE',  #5892 ) ;
#25963 = SPHERICAL_SURFACE ( 'NONE', #18959, 35.18636678425505693 ) ;
#25964 = VECTOR ( 'NONE', #17998, 1000.000000000000000 ) ;
#25965 = VERTEX_POINT ( 'NONE', #18041 ) ;
#25966 = DIRECTION ( 'NONE',  ( -0.8916010070293383105, -0.4528218681383106015, 0.000000000000000000 ) ) ;
#25967 = PLANE ( 'NONE',  #21774 ) ;
#25968 = DIRECTION ( 'NONE',  ( -0.8916010070293383105, -0.4528218681383106015, 0.000000000000000000 ) ) ;
#25969 = VECTOR ( 'NONE', #2560, 1000.000000000000000 ) ;
#25971 = VERTEX_POINT ( 'NONE', #20476 ) ;
#25970 = EDGE_LOOP ( 'NONE', ( #1054, #26605, #26752, #24753, #10403, #2391, #786, #8032 ) ) ;
#25972 = CARTESIAN_POINT ( 'NONE',  ( 91.79864198314089663, 239.6982472080514128, -17.32810371388483262 ) ) ;
#25973 = ORIENTED_EDGE ( 'NONE', *, *, #2567, .F. ) ;
#25974 = EDGE_LOOP ( 'NONE', ( #18127, #27659, #17009, #17248 ) ) ;
#25975 = ORIENTED_EDGE ( 'NONE', *, *, #5223, .F. ) ;
#25976 = ORIENTED_EDGE ( 'NONE', *, *, #23762, .F. ) ;
#25977 = ORIENTED_EDGE ( 'NONE', *, *, #14866, .F. ) ;
#25978 = ORIENTED_EDGE ( 'NONE', *, *, #19903, .T. ) ;
#25979 = VECTOR ( 'NONE', #25302, 1000.000000000000114 ) ;
#25980 = CARTESIAN_POINT ( 'NONE',  ( 134.9999999999998579, 404.6636166603179277, -152.9999999999999716 ) ) ;
#25981 = EDGE_CURVE ( 'NONE', #23466, #24318, #13639, .T. ) ;
#25982 = DIRECTION ( 'NONE',  ( -0.8916010070298968637, -0.4528218681372109811, 0.000000000000000000 ) ) ;
#25983 = VECTOR ( 'NONE', #18344, 1000.000000000000000 ) ;
#25984 = DIRECTION ( 'NONE',  ( 0.000000000000000000, 0.000000000000000000, -1.000000000000000000 ) ) ;
#25985 = DIRECTION ( 'NONE',  ( 1.000000000000000000, -0.000000000000000000, -0.000000000000000000 ) ) ;
#25986 = EDGE_CURVE ( 'NONE', #1215, #14420, #11871, .T. ) ;
#25987 = DIRECTION ( 'NONE',  ( -0.4528218681383003319, -0.8916010070293436396, 0.000000000000000000 ) ) ;
#25988 = CARTESIAN_POINT ( 'NONE',  ( 157.4999999999998579, 221.2539375037535194, 45.00000000000000000 ) ) ;
#25989 = DIRECTION ( 'NONE',  ( -1.000000000000000000, -1.530283246943720875E-16, 0.000000000000000000 ) ) ;
#25990 = EDGE_CURVE ( 'NONE', #27621, #25194, #26800, .T. ) ;
#25991 = CARTESIAN_POINT ( 'NONE',  ( -24.64763201754189481, 128.0468424616478273, 17.48411470635667797 ) ) ;
#25992 = CARTESIAN_POINT ( 'NONE',  ( -209.9392250573528429, 62.66900426808626179, 27.74467448083618493 ) ) ;
#25993 = DIRECTION ( 'NONE',  ( 0.8916010070317489378, -0.4528218681335642315, 0.000000000000000000 ) ) ;
#25994 = DIRECTION ( 'NONE',  ( 1.000000000000000000, 0.000000000000000000, 0.000000000000000000 ) ) ;
#25995 = VERTEX_POINT ( 'NONE', #9704 ) ;
#25996 = CIRCLE ( 'NONE', #10860, 5.000000000000004441 ) ;
#25997 = CARTESIAN_POINT ( 'NONE',  ( -188.6435715486210540, 104.1343366490829823, 32.77691502914932897 ) ) ;
#25998 = CARTESIAN_POINT ( 'NONE',  ( -271.7051148791218793, -170.2004882804717738, -108.6368843222754066 ) ) ;
#25999 = VERTEX_POINT ( 'NONE', #2801 ) ;
#26000 = ORIENTED_EDGE ( 'NONE', *, *, #24863, .F. ) ;
#26001 = EDGE_CURVE ( 'NONE', #24382, #8538, #24648, .T. ) ;
#26002 = EDGE_LOOP ( 'NONE', ( #3897, #1112 ) ) ;
#26003 = CARTESIAN_POINT ( 'NONE',  ( -217.7401460507883826, 138.5677444271665877, -12.99353264133693919 ) ) ;
#26004 = FACE_OUTER_BOUND ( 'NONE', #2110, .T. ) ;
#26005 = VERTEX_POINT ( 'NONE', #4951 ) ;
#26006 = ORIENTED_EDGE ( 'NONE', *, *, #11489, .F. ) ;
#26007 = CARTESIAN_POINT ( 'NONE',  ( 108.2273028572353297, 129.5338070842080924, -88.59375000024363089 ) ) ;
#26008 = EDGE_CURVE ( 'NONE', #21355, #16933, #18465, .T. ) ;
#26009 = DIRECTION ( 'NONE',  ( 0.000000000000000000, 0.000000000000000000, 1.000000000000000000 ) ) ;
#26010 = PLANE ( 'NONE',  #2703 ) ;
#26011 = EDGE_LOOP ( 'NONE', ( #15261, #4443, #16664, #24387 ) ) ;
#26012 = CARTESIAN_POINT ( 'NONE',  ( -222.3308448878950401, 86.50594421447330262, 17.61308416972892132 ) ) ;
#26013 = VERTEX_POINT ( 'NONE', #18191 ) ;
#26014 = VECTOR ( 'NONE', #17853, 1000.000000000000000 ) ;
#26015 = FACE_OUTER_BOUND ( 'NONE', #1732, .T. ) ;
#26016 = CLOSED_SHELL ( 'NONE', ( #13653, #19303, #16720, #28367, #4068, #5747, #23712, #11083, #13482, #27533, #17092, #15272, #4066, #20793, #24131, #23555, #20154, #11984, #8451, #20780, #26839, #11175, #4283, #20986, #3600, #25153 ) ) ;
#26017 = CARTESIAN_POINT ( 'NONE',  ( 217.4999999999996305, 133.0668745871126930, 30.86484227207697018 ) ) ;
#26018 = CARTESIAN_POINT ( 'NONE',  ( 160.9807621135329612, 204.9999999999999147, -138.9999999999999432 ) ) ;
#26019 = LINE ( 'NONE', #425, #1419 ) ;
#26020 = ORIENTED_EDGE ( 'NONE', *, *, #13685, .T. ) ;
#26021 = EDGE_CURVE ( 'NONE', #9499, #8677, #16321, .T. ) ;
#26022 = ADVANCED_FACE ( 'NONE', ( #1076 ), #9844, .F. ) ;
#26023 = CARTESIAN_POINT ( 'NONE',  ( 153.4775906502256930, 212.3463313526982859, -45.00000000000000000 ) ) ;
#26024 = DIRECTION ( 'NONE',  ( 1.000000000000000000, 0.000000000000000000, -0.000000000000000000 ) ) ;
#26025 = LINE ( 'NONE', #24029, #571 ) ;
#26026 = DIRECTION ( 'NONE',  ( -0.8916010070299376089, -0.4528218681371311005, 0.000000000000000000 ) ) ;
#26027 = EDGE_LOOP ( 'NONE', ( #26598, #16936, #2540, #20843 ) ) ;
#26028 = CARTESIAN_POINT ( 'NONE',  ( 157.4999999999998579, 186.1436873986549188, 45.00000000000000000 ) ) ;
#26029 = AXIS2_PLACEMENT_3D ( 'NONE', #25011, #4892, #22853 ) ;
#26030 = DIRECTION ( 'NONE',  ( 0.4528218681370523302, 0.8916010070299774659, -0.000000000000000000 ) ) ;
#26031 = CARTESIAN_POINT ( 'NONE',  ( 157.9999999999996874, 268.6496251426330559, 45.00000000000000000 ) ) ;
#26032 = CARTESIAN_POINT ( 'NONE',  ( 134.9999999999998579, 433.5940952139197293, -145.0000000000000000 ) ) ;
#26033 = VERTEX_POINT ( 'NONE', #15756 ) ;
#26034 =( LENGTH_UNIT ( ) NAMED_UNIT ( * ) SI_UNIT ( .MILLI., .METRE. ) );
#26035 = LINE ( 'NONE', #6356, #6082 ) ;
#26036 = ORIENTED_EDGE ( 'NONE', *, *, #21618, .T. ) ;
#26037 = AXIS2_PLACEMENT_3D ( 'NONE', #11188, #26397, #6724 ) ;
#26038 = EDGE_CURVE ( 'NONE', #11330, #5169, #24505, .T. ) ;
#26039 = EDGE_CURVE ( 'NONE', #2675, #5984, #22349, .T. ) ;
#26040 = FACE_OUTER_BOUND ( 'NONE', #17637, .T. ) ;
#26041 = CARTESIAN_POINT ( 'NONE',  ( -167.8789958130436162, 116.8334710968284327, -25.29509310206942985 ) ) ;
#26042 = ORIENTED_EDGE ( 'NONE', *, *, #1911, .F. ) ;
#26043 = VERTEX_POINT ( 'NONE', #25762 ) ;
#26044 = CARTESIAN_POINT ( 'NONE',  ( -112.9862511722770790, 70.97208026367574973, 82.84066614128462902 ) ) ;
#26045 = ORIENTED_EDGE ( 'NONE', *, *, #1779, .T. ) ;
#26046 = CARTESIAN_POINT ( 'NONE',  ( 158.0000000000017337, 40.94087446699997912, 45.00000000000000000 ) ) ;
#26047 = ADVANCED_FACE ( 'NONE', ( #6087 ), #8247, .F. ) ;
#26048 = VERTEX_POINT ( 'NONE', #25487 ) ;
#26049 = VERTEX_POINT ( 'NONE', #14721 ) ;
#26050 = DIRECTION ( 'NONE',  ( 0.000000000000000000, 0.000000000000000000, -1.000000000000000000 ) ) ;
#26051 = TOROIDAL_SURFACE ( 'NONE', #1285, 68.83858790703926900, 2.000000000000000000 ) ;
#26052 = VECTOR ( 'NONE', #10105, 1000.000000000000000 ) ;
#26053 = DIRECTION ( 'NONE',  ( 0.000000000000000000, 0.000000000000000000, -1.000000000000000000 ) ) ;
#26054 = DIRECTION ( 'NONE',  ( -1.000000000000000000, 0.000000000000000000, 0.000000000000000000 ) ) ;
#26055 = CARTESIAN_POINT ( 'NONE',  ( 158.0000000000008811, 121.1928747072253572, 45.00000000000000000 ) ) ;
#26056 = CARTESIAN_POINT ( 'NONE',  ( -268.0136499788973765, -170.6190998804379717, 104.4234267195772219 ) ) ;
#26057 = LINE ( 'NONE', #8820, #14941 ) ;
#26058 = CARTESIAN_POINT ( 'NONE',  ( -228.6046226639666088, 73.96500373646588855, -16.69423931604977085 ) ) ;
#26059 = EDGE_LOOP ( 'NONE', ( #13745, #14362, #15071, #1693 ) ) ;
#26060 = DIRECTION ( 'NONE',  ( 0.8660254037844432595, 0.4999999999999919509, -0.000000000000000000 ) ) ;
#26061 = CARTESIAN_POINT ( 'NONE',  ( 158.0000000000006253, 148.2716247822957882, -45.00000000000000000 ) ) ;
#26062 = CARTESIAN_POINT ( 'NONE',  ( 156.4999999999998579, 220.0000000000000284, 100.0000000000000142 ) ) ;
#26063 = CARTESIAN_POINT ( 'NONE',  ( 113.4521041897134097, 213.5046054548297434, -97.56026172913361449 ) ) ;
#26064 = ORIENTED_EDGE ( 'NONE', *, *, #4505, .F. ) ;
#26065 = CARTESIAN_POINT ( 'NONE',  ( -226.5998460896583993, 62.96930358458836707, 8.263950894743116393 ) ) ;
#26066 = AXIS2_PLACEMENT_3D ( 'NONE', #7714, #14323, #5695 ) ;
#26067 = DIRECTION ( 'NONE',  ( 0.8916010070295011802, 0.4528218681379903021, 0.000000000000000000 ) ) ;
#26068 = DIRECTION ( 'NONE',  ( 0.000000000000000000, -0.000000000000000000, -1.000000000000000000 ) ) ;
#26069 = CARTESIAN_POINT ( 'NONE',  ( 145.6339745962154097, 240.4185842870418242, 45.00000000000000000 ) ) ;
#26070 = DIRECTION ( 'NONE',  ( -0.2588190451025286221, -0.9659258262890662028, 0.000000000000000000 ) ) ;
#26071 = CARTESIAN_POINT ( 'NONE',  ( 134.9999999999998579, 220.0000000000000284, 100.0000000000000142 ) ) ;
#26072 = VERTEX_POINT ( 'NONE', #7690 ) ;
#26073 = CARTESIAN_POINT ( 'NONE',  ( -231.4586860447602703, 76.02675087360279349, 15.76935333479230117 ) ) ;
#26074 = ORIENTED_EDGE ( 'NONE', *, *, #8028, .F. ) ;
#26075 = DIRECTION ( 'NONE',  ( 0.6681556583950049033, -0.7440215159219103480, 0.000000000000000000 ) ) ;
#26076 = VECTOR ( 'NONE', #14005, 1000.000000000000114 ) ;
#26077 = EDGE_LOOP ( 'NONE', ( #2053, #1489, #23419, #4348 ) ) ;
#26078 = ORIENTED_EDGE ( 'NONE', *, *, #21438, .F. ) ;
#26079 = EDGE_CURVE ( 'NONE', #16458, #10433, #1217, .T. ) ;
#26080 = CARTESIAN_POINT ( 'NONE',  ( -200.0000000000000284, 0.000000000000000000, 25.00000000000000000 ) ) ;
#26081 = ORIENTED_EDGE ( 'NONE', *, *, #26497, .F. ) ;
#26082 = ORIENTED_EDGE ( 'NONE', *, *, #17635, .T. ) ;
#26083 = CARTESIAN_POINT ( 'NONE',  ( -224.3418196798764086, 136.6081117166938839, 14.97424725141357271 ) ) ;
#26084 = CARTESIAN_POINT ( 'NONE',  ( 115.5814157129579058, 207.6339745962153245, 45.00000000000000000 ) ) ;
#26085 = CARTESIAN_POINT ( 'NONE',  ( 158.0000000000008527, 125.7007497147323818, 45.00000000000000000 ) ) ;
#26086 = LINE ( 'NONE', #23946, #21806 ) ;
#26087 = PLANE ( 'NONE',  #892 ) ;
#26088 = CARTESIAN_POINT ( 'NONE',  ( -12.24491960465745599, 29.64876300893806516, 95.00000000000000000 ) ) ;
#26089 = VECTOR ( 'NONE', #26624, 1000.000000000000114 ) ;
#26090 = DIRECTION ( 'NONE',  ( 0.000000000000000000, 0.000000000000000000, 1.000000000000000000 ) ) ;
#26091 = CARTESIAN_POINT ( 'NONE',  ( 158.0000000000005969, 150.7794997898028271, 45.00000000000000000 ) ) ;
#26092 = LINE ( 'NONE', #13326, #8067 ) ;
#26093 = VECTOR ( 'NONE', #14277, 1000.000000000000000 ) ;
#26094 = DIRECTION ( 'NONE',  ( 0.4528218681370324572, 0.8916010070299876800, -0.000000000000000000 ) ) ;
#26095 = CARTESIAN_POINT ( 'NONE',  ( 432.4999999999996589, 0.000000000000000000, 0.000000000000000000 ) ) ;
#26096 = CARTESIAN_POINT ( 'NONE',  ( 109.9999999999999147, 140.0000000000000000, -90.00000000000004263 ) ) ;
#26097 = DIRECTION ( 'NONE',  ( 0.8018642810807398158, 0.5975062131282554700, 0.000000000000000000 ) ) ;
#26098 = ORIENTED_EDGE ( 'NONE', *, *, #22661, .F. ) ;
#26099 = FACE_OUTER_BOUND ( 'NONE', #8992, .T. ) ;
#26100 = VECTOR ( 'NONE', #4887, 1000.000000000000114 ) ;
#26101 = EDGE_CURVE ( 'NONE', #22270, #25748, #9305, .T. ) ;
#26102 = DIRECTION ( 'NONE',  ( 0.000000000000000000, 0.000000000000000000, 1.000000000000000000 ) ) ;
#26103 = DIRECTION ( 'NONE',  ( 1.000000000000000000, 0.000000000000000000, 0.000000000000000000 ) ) ;
#26104 = CARTESIAN_POINT ( 'NONE',  ( 106.8096100835816458, 209.7359181041861689, -148.0084258618598199 ) ) ;
#26105 = VERTEX_POINT ( 'NONE', #23055 ) ;
#26106 = CIRCLE ( 'NONE', #23824, 1.000000000000000888 ) ;
#26107 = CARTESIAN_POINT ( 'NONE',  ( 88.62124187923063801, 239.8086506234227784, -16.24979138472547291 ) ) ;
#26108 = ORIENTED_EDGE ( 'NONE', *, *, #6149, .F. ) ;
#26109 = ORIENTED_EDGE ( 'NONE', *, *, #830, .F. ) ;
#26110 = CIRCLE ( 'NONE', #20104, 22.49999999999999289 ) ;
#26111 = EDGE_CURVE ( 'NONE', #20930, #15999, #23196, .T. ) ;
#26112 = VERTEX_POINT ( 'NONE', #3505 ) ;
#26113 = ADVANCED_FACE ( 'NONE', ( #10267 ), #10404, .F. ) ;
#26114 = EDGE_CURVE ( 'NONE', #24909, #13241, #27488, .T. ) ;
#26115 = AXIS2_PLACEMENT_3D ( 'NONE', #1411, #27964, #3699 ) ;
#26116 = ADVANCED_FACE ( 'NONE', ( #3647 ), #19110, .T. ) ;
#26117 = ORIENTED_EDGE ( 'NONE', *, *, #25535, .F. ) ;
#26118 = VERTEX_POINT ( 'NONE', #3364 ) ;
#26119 = VERTEX_POINT ( 'NONE', #1358 ) ;
#26120 = DIRECTION ( 'NONE',  ( -1.000000000000000000, 0.000000000000000000, 0.000000000000000000 ) ) ;
#26121 = VECTOR ( 'NONE', #16668, 999.9999999999998863 ) ;
#26122 = FACE_OUTER_BOUND ( 'NONE', #7884, .T. ) ;
#26123 = UNCERTAINTY_MEASURE_WITH_UNIT (LENGTH_MEASURE( 1.000000000000000082E-05 ), #24822, 'distance_accuracy_value', 'NONE');
#26124 = CARTESIAN_POINT ( 'NONE',  ( 150.8670668058247202, 207.8247714198255949, 45.00000000000000000 ) ) ;
#26125 = LINE ( 'NONE', #2271, #18398 ) ;
#26126 = PLANE ( 'NONE',  #8988 ) ;
#26127 = CIRCLE ( 'NONE', #13772, 7.499999999999992895 ) ;
#26128 = CARTESIAN_POINT ( 'NONE',  ( -40.77202656396519131, 129.1845453850527576, -17.01159430929711291 ) ) ;
#26129 = FACE_OUTER_BOUND ( 'NONE', #6411, .T. ) ;
#26130 = B_SPLINE_CURVE_WITH_KNOTS ( 'NONE', 3,
 ( #28223, #26491, #6823, #4519, #15180, #24078, #8566, #26217 ),
 .UNSPECIFIED., .F., .F.,
 ( 4, 2, 2, 4 ),
 ( 0.000000000000000000, 0.009823234264782376712, 0.01473485139717357027, 0.01964646852956476383 ),
 .UNSPECIFIED. ) ;
#26131 = DIRECTION ( 'NONE',  ( -0.000000000000000000, -0.000000000000000000, -1.000000000000000000 ) ) ;
#26132 = LINE ( 'NONE', #19810, #27639 ) ;
#26133 = AXIS2_PLACEMENT_3D ( 'NONE', #26519, #19781, #106 ) ;
#26134 = CARTESIAN_POINT ( 'NONE',  ( 109.2179431711400639, 204.6558323512134621, -151.0000000000000853 ) ) ;
#26135 = CYLINDRICAL_SURFACE ( 'NONE', #9630, 58.59270260175150469 ) ;
#26136 = CARTESIAN_POINT ( 'NONE',  ( 217.4999999999996305, 133.0668745871126930, 36.86484227207694886 ) ) ;
#26137 = FACE_OUTER_BOUND ( 'NONE', #27687, .T. ) ;
#26139 = ORIENTED_EDGE ( 'NONE', *, *, #24, .T. ) ;
#26138 = ORIENTED_EDGE ( 'NONE', *, *, #514, .T. ) ;
#26140 = CARTESIAN_POINT ( 'NONE',  ( -226.9732155144656360, 87.81596337922499629, -15.90667162794334466 ) ) ;
#26141 = EDGE_CURVE ( 'NONE', #506, #12924, #14443, .T. ) ;
#26142 = EDGE_CURVE ( 'NONE', #11731, #1736, #19023, .T. ) ;
#26143 = CARTESIAN_POINT ( 'NONE',  ( -275.9276330244907172, -170.0000000000001137, -102.1496523160547838 ) ) ;
#26144 = VERTEX_POINT ( 'NONE', #27768 ) ;
#26145 = PRODUCT_CONTEXT ( 'NONE', #18281, 'mechanical' ) ;
#26146 = ORIENTED_EDGE ( 'NONE', *, *, #9614, .F. ) ;
#26147 = ORIENTED_EDGE ( 'NONE', *, *, #27368, .T. ) ;
#26148 = CARTESIAN_POINT ( 'NONE',  ( 65.00000000000000000, -120.0250000000000625, 64.00000000000001421 ) ) ;
#26149 = VECTOR ( 'NONE', #13608, 1000.000000000000000 ) ;
#26150 = DIRECTION ( 'NONE',  ( 0.4528218681383305855, -0.8916010070293283185, 0.000000000000000000 ) ) ;
#26151 = EDGE_CURVE ( 'NONE', #16250, #8798, #20895, .T. ) ;
#26152 = ORIENTED_EDGE ( 'NONE', *, *, #4570, .F. ) ;
#26153 = CARTESIAN_POINT ( 'NONE',  ( 109.6721745451464045, 96.60743919220468001, -100.0000000000000142 ) ) ;
#26154 = VECTOR ( 'NONE', #4052, 1000.000000000000114 ) ;
#26155 =( REPRESENTATION_RELATIONSHIP ('NONE','NONE', #11963, #14145 ) REPRESENTATION_RELATIONSHIP_WITH_TRANSFORMATION ( #6748 )SHAPE_REPRESENTATION_RELATIONSHIP( ) );
#26156 = FACE_OUTER_BOUND ( 'NONE', #12417, .T. ) ;
#26157 = ORIENTED_EDGE ( 'NONE', *, *, #9136, .T. ) ;
#26158 = CARTESIAN_POINT ( 'NONE',  ( -215.0606129237200719, 86.58168940511831124, 21.65971791556373205 ) ) ;
#26159 = ORIENTED_EDGE ( 'NONE', *, *, #8286, .T. ) ;
#26160 = FACE_OUTER_BOUND ( 'NONE', #27220, .T. ) ;
#26161 = B_SPLINE_CURVE_WITH_KNOTS ( 'NONE', 3,
 ( #715, #5155, #2565, #26851, #4576, #9483, #22692, #26550, #17797, #18238, #20239, #18379, #11788, #20526, #15812, #13362, #851, #15948, #7319, #5007, #11202, #9335 ),
 .UNSPECIFIED., .F., .F.,
 ( 4, 2, 2, 2, 2, 2, 2, 2, 2, 2, 4 ),
 ( 0.000000000000000000, 0.1250000000000000000, 0.2500000000000000000, 0.3750000000000000000, 0.5000000000000000000, 0.6250000000000000000, 0.7500000000000000000, 0.8125000000000000000, 0.8750000000000001110, 0.9375000000000001110, 1.000000000000000000 ),
 .UNSPECIFIED. ) ;
#26162 = DIRECTION ( 'NONE',  ( -0.9586565047779721516, -0.2845658198851048759, 0.000000000000000000 ) ) ;
#26163 = DIRECTION ( 'NONE',  ( 1.000000000000000000, -0.000000000000000000, -0.000000000000000000 ) ) ;
#26164 = DIRECTION ( 'NONE',  ( -0.000000000000000000, -0.000000000000000000, 1.000000000000000000 ) ) ;
#26165 = ORIENTED_EDGE ( 'NONE', *, *, #15183, .F. ) ;
#26166 = VECTOR ( 'NONE', #14589, 1000.000000000000000 ) ;
#26167 = CARTESIAN_POINT ( 'NONE',  ( 118.3245732435417068, 204.8512006320913486, 99.88685888571269800 ) ) ;
#26168 = CARTESIAN_POINT ( 'NONE',  ( 157.4999999999998579, 146.0176872785422404, 45.00000000000000000 ) ) ;
#26169 = DIRECTION ( 'NONE',  ( -0.8916010070299679180, -0.4528218681370710375, 0.000000000000000000 ) ) ;
#26170 = CARTESIAN_POINT ( 'NONE',  ( -63.57415822541634043, -18.01420295945611727, 95.00000000000000000 ) ) ;
#26171 = ORIENTED_EDGE ( 'NONE', *, *, #16147, .F. ) ;
#26172 = PLANE ( 'NONE',  #8708 ) ;
#26173 = CIRCLE ( 'NONE', #9210, 21.49999999999997868 ) ;
#26174 = ADVANCED_FACE ( 'NONE', ( #7825 ), #5946, .F. ) ;
#26175 = DIRECTION ( 'NONE',  ( 1.000000000000000000, 2.602085213965211135E-16, -0.000000000000000000 ) ) ;
#26176 = B_SPLINE_CURVE_WITH_KNOTS ( 'NONE', 3,
 ( #13825, #2885, #9506, #7348, #9644, #3154, #18401, #5322, #27151, #16392, #11946, #5456, #14240, #22990, #16257, #3293, #20685, #20830, #9922, #18675, #7056, #15838, #21532, #14943, #25280, #16807, #25422, #5600, #12505, #18813, #5879, #16670, #7763, #18960, #7897, #25554, #25842, #8041 ),
 .UNSPECIFIED., .F., .F.,
 ( 4, 2, 2, 2, 2, 2, 2, 2, 2, 2, 2, 2, 2, 2, 2, 2, 2, 2, 4 ),
 ( 0.000000000000000000, 0.003178314472605698292, 0.004767471708908553943, 0.006356628945211410461, 0.007945786181514265245, 0.009534943417817123498, 0.01271325789042283480, 0.01430241512672566877, 0.01589157236302849927, 0.01906988683563421577, 0.02542651578084565225, 0.02860483025345133060, 0.03178314472605699853, 0.03813977367126838991, 0.04449640261647971884, 0.04767471708908538330, 0.04926387432538828492, 0.05005845294353974267, 0.05085303156169119349 ),
 .UNSPECIFIED. ) ;
#26177 = DIRECTION ( 'NONE',  ( 1.000000000000000000, 0.000000000000000000, 0.000000000000000000 ) ) ;
#26178 = VERTEX_POINT ( 'NONE', #21316 ) ;
#26179 = ORIENTED_EDGE ( 'NONE', *, *, #19794, .T. ) ;
#26180 = LINE ( 'NONE', #17997, #554 ) ;
#26181 = CARTESIAN_POINT ( 'NONE',  ( -187.3254023397375363, 105.2541933103603782, -31.76634463011786380 ) ) ;
#26182 = ORIENTED_EDGE ( 'NONE', *, *, #10352, .T. ) ;
#26183 = ORIENTED_EDGE ( 'NONE', *, *, #17947, .F. ) ;
#26184 = FACE_OUTER_BOUND ( 'NONE', #13742, .T. ) ;
#26185 = EDGE_CURVE ( 'NONE', #230, #5960, #769, .T. ) ;
#26186 = VECTOR ( 'NONE', #14557, 1000.000000000000000 ) ;
#26187 = EDGE_CURVE ( 'NONE', #20000, #21343, #1633, .T. ) ;
#26188 = ORIENTED_EDGE ( 'NONE', *, *, #11307, .T. ) ;
#26189 = ORIENTED_EDGE ( 'NONE', *, *, #18044, .F. ) ;
#26190 = CARTESIAN_POINT ( 'NONE',  ( -3.611973201795212418, 132.7557511336061395, 15.88408374257556055 ) ) ;
#26191 = AXIS2_PLACEMENT_3D ( 'NONE', #4155, #8623, #17373 ) ;
#26192 = CARTESIAN_POINT ( 'NONE',  ( 158.0000000000016200, 50.97237449702815582, 45.00000000000000000 ) ) ;
#26193 = CARTESIAN_POINT ( 'NONE',  ( -225.7036482868739427, -91.18033988749901653, -18.91107291867258766 ) ) ;
#26194 = CARTESIAN_POINT ( 'NONE',  ( 330.9869376377542949, 44.41075299063185611, -75.35061095560293154 ) ) ;
#26195 = EDGE_CURVE ( 'NONE', #12815, #5308, #19300, .T. ) ;
#26196 = CARTESIAN_POINT ( 'NONE',  ( -210.0000000000000000, -150.0000000000001990, 100.0000000000000142 ) ) ;
#26197 = DIRECTION ( 'NONE',  ( 0.8916010070297643031, -0.4528218681374719945, 0.000000000000000000 ) ) ;
#26198 = VERTEX_POINT ( 'NONE', #15145 ) ;
#26199 = ADVANCED_FACE ( 'NONE', ( #4208 ), #17708, .F. ) ;
#26200 = CARTESIAN_POINT ( 'NONE',  ( -2.862293735361731706E-14, 109.9999999999999858, 100.0000000000000142 ) ) ;
#26201 = FACE_OUTER_BOUND ( 'NONE', #22080, .T. ) ;
#26202 = CARTESIAN_POINT ( 'NONE',  ( 158.0000000000009095, 120.6849996997183183, 45.00000000000000000 ) ) ;
#26203 = CARTESIAN_POINT ( 'NONE',  ( 113.5875366493131509, 226.9823751442990840, -97.68174538100610960 ) ) ;
#26204 = ORIENTED_EDGE ( 'NONE', *, *, #23067, .T. ) ;
#26205 = DIRECTION ( 'NONE',  ( -1.000000000000000000, -0.000000000000000000, -0.000000000000000000 ) ) ;
#26206 = B_SPLINE_CURVE_WITH_KNOTS ( 'NONE', 3,
 ( #20520, #844, #7457, #16226, #21080, #14211 ),
 .UNSPECIFIED., .F., .F.,
 ( 4, 2, 4 ),
 ( 0.000000000000000000, 0.004615224477119856013, 0.009230448954239712026 ),
 .UNSPECIFIED. ) ;
#26207 = AXIS2_PLACEMENT_3D ( 'NONE', #15345, #26375, #15916 ) ;
#26208 = CARTESIAN_POINT ( 'NONE',  ( -77.29631966220712513, 4.740818392941735127, -15.00000000000000000 ) ) ;
#26209 = CARTESIAN_POINT ( 'NONE',  ( 157.9999999999998295, 231.0315000300280417, 45.00000000000000000 ) ) ;
#26210 = FACE_OUTER_BOUND ( 'NONE', #26941, .T. ) ;
#26211 = LINE ( 'NONE', #22049, #1438 ) ;
#26212 = DIRECTION ( 'NONE',  ( 1.000000000000000000, -0.000000000000000000, -0.000000000000000000 ) ) ;
#26213 = ORIENTED_EDGE ( 'NONE', *, *, #20063, .T. ) ;
#26214 = VECTOR ( 'NONE', #6152, 1000.000000000000000 ) ;
#26215 = CARTESIAN_POINT ( 'NONE',  ( -229.0277751032626838, 74.22523041939535915, 16.53402846819822614 ) ) ;
#26216 = EDGE_LOOP ( 'NONE', ( #25270, #18664, #11301, #1251 ) ) ;
#26217 = CARTESIAN_POINT ( 'NONE',  ( -260.0000000000001137, -167.0819201924624906, 110.0000000000000142 ) ) ;
#26218 = VERTEX_POINT ( 'NONE', #28325 ) ;
#26219 = ORIENTED_EDGE ( 'NONE', *, *, #15059, .T. ) ;
#26220 = EDGE_CURVE ( 'NONE', #26801, #27657, #4423, .T. ) ;
#26221 = CARTESIAN_POINT ( 'NONE',  ( 157.4999999999998579, 188.6515624061619576, 45.00000000000000000 ) ) ;
#26222 = EDGE_CURVE ( 'NONE', #28003, #21880, #8393, .T. ) ;
#26223 = EDGE_LOOP ( 'NONE', ( #25419, #23495, #20960, #21096 ) ) ;
#26224 = ORIENTED_EDGE ( 'NONE', *, *, #2678, .F. ) ;
#26225 = DIRECTION ( 'NONE',  ( 0.000000000000000000, 0.000000000000000000, 1.000000000000000000 ) ) ;
#26226 = DIRECTION ( 'NONE',  ( -0.9784193629480781862, 0.2066290158914688424, 0.000000000000000000 ) ) ;
#26227 = CARTESIAN_POINT ( 'NONE',  ( 157.4999999999998579, 220.0000000000000284, 100.0000000000000142 ) ) ;
#26228 = AXIS2_PLACEMENT_3D ( 'NONE', #24063, #15310, #2487 ) ;
#26229 = CARTESIAN_POINT ( 'NONE',  ( 158.0000000000001137, 193.9212499249295831, -45.00000000000000000 ) ) ;
#26230 = DIRECTION ( 'NONE',  ( 1.000000000000000000, 0.000000000000000000, 0.000000000000000000 ) ) ;
#26231 = AXIS2_PLACEMENT_3D ( 'NONE', #11690, #18559, #20707 ) ;
#26232 = AXIS2_PLACEMENT_3D ( 'NONE', #19857, #184, #9232 ) ;
#26233 = EDGE_CURVE ( 'NONE', #24201, #20577, #318, .T. ) ;
#26234 = AXIS2_PLACEMENT_3D ( 'NONE', #18033, #25197, #929 ) ;
#26235 = CARTESIAN_POINT ( 'NONE',  ( 127.3463313526980727, 238.4775906502252667, 45.00000000000000000 ) ) ;
#26236 = CARTESIAN_POINT ( 'NONE',  ( 157.4999999999998579, 220.0000000000000284, -105.0000000000000284 ) ) ;
#26237 = CARTESIAN_POINT ( 'NONE',  ( -209.0446251875730752, 89.43114028902917312, -24.28448859940165860 ) ) ;
#26238 = CARTESIAN_POINT ( 'NONE',  ( 217.4999999999996305, 258.6181251126050711, 1.387778780781445676E-14 ) ) ;
#26239 = LINE ( 'NONE', #6566, #12654 ) ;
#26240 = CARTESIAN_POINT ( 'NONE',  ( 157.9999999999996874, 269.1575001501400379, 45.00000000000000000 ) ) ;
#26241 = CARTESIAN_POINT ( 'NONE',  ( 367.4999999999996021, 44.41075299063183479, 100.0000000000000284 ) ) ;
#26242 = DIRECTION ( 'NONE',  ( -1.000000000000000000, 0.000000000000000000, 0.000000000000000000 ) ) ;
#26243 = EDGE_CURVE ( 'NONE', #226, #19699, #4063, .T. ) ;
#26244 = ORIENTED_EDGE ( 'NONE', *, *, #12385, .F. ) ;
#26245 = CYLINDRICAL_SURFACE ( 'NONE', #14727, 2.000000000000000000 ) ;
#26246 = EDGE_CURVE ( 'NONE', #12221, #24936, #11798, .T. ) ;
#26247 = CARTESIAN_POINT ( 'NONE',  ( 112.0033315760181267, 140.0000000000000000, 96.14546719974917721 ) ) ;
#26248 = CARTESIAN_POINT ( 'NONE',  ( 134.9999999999998579, 220.0000000000000284, -169.9999999999999716 ) ) ;
#26249 = ADVANCED_FACE ( 'NONE', ( #26184 ), #46, .T. ) ;
#26250 = DIRECTION ( 'NONE',  ( 0.4528218681371523058, 0.8916010070299268397, -0.000000000000000000 ) ) ;
#26251 = ORIENTED_EDGE ( 'NONE', *, *, #2934, .F. ) ;
#26252 = VECTOR ( 'NONE', #19996, 1000.000000000000114 ) ;
#26253 = TOROIDAL_SURFACE ( 'NONE', #7899, 72.21503689626331379, 5.000000000000000000 ) ;
#26254 = CARTESIAN_POINT ( 'NONE',  ( -175.0000000000000000, -120.0250000000001762, 76.00000000000002842 ) ) ;
#26255 = ORIENTED_EDGE ( 'NONE', *, *, #27103, .F. ) ;
#26256 = CARTESIAN_POINT ( 'NONE',  ( -1.286675988402057991, 135.5503650875635344, -13.59707690229856247 ) ) ;
#26257 = EDGE_LOOP ( 'NONE', ( #21019, #21240, #25385, #4518 ) ) ;
#26258 = AXIS2_PLACEMENT_3D ( 'NONE', #9204, #13667, #16106 ) ;
#26259 = VERTEX_POINT ( 'NONE', #17285 ) ;
#26260 = VECTOR ( 'NONE', #25479, 1000.000000000000000 ) ;
#26261 = ORIENTED_EDGE ( 'NONE', *, *, #3680, .F. ) ;
#26262 = ORIENTED_EDGE ( 'NONE', *, *, #9711, .T. ) ;
#26263 = ORIENTED_EDGE ( 'NONE', *, *, #3358, .F. ) ;
#26264 = CARTESIAN_POINT ( 'NONE',  ( -10.78991826960876033, 200.8449754580304898, 45.00000000000000000 ) ) ;
#26265 = CARTESIAN_POINT ( 'NONE',  ( 349.0018770490532916, 96.44595867864242678, -134.2811822434183853 ) ) ;
#26266 = DIRECTION ( 'NONE',  ( 0.8379557447115514313, -0.5457381880580733924, 0.000000000000000000 ) ) ;
#26267 = TOROIDAL_SURFACE ( 'NONE', #25798, 7.509856658345970715, 10.53396790234564762 ) ;
#26268 = CARTESIAN_POINT ( 'NONE',  ( -215.3445465745180343, 71.74628434702681545, 26.24848034640717032 ) ) ;
#26269 = CARTESIAN_POINT ( 'NONE',  ( 157.9999999999998579, 221.0000000000000284, -45.00000000000000000 ) ) ;
#26270 = DIRECTION ( 'NONE',  ( 0.8916010070293783896, 0.4528218681382319422, 0.000000000000000000 ) ) ;
#26271 = VECTOR ( 'NONE', #4441, 1000.000000000000000 ) ;
#26272 = DIRECTION ( 'NONE',  ( -0.000000000000000000, -1.000000000000000000, -0.000000000000000000 ) ) ;
#26273 = DIRECTION ( 'NONE',  ( -0.000000000000000000, -0.000000000000000000, -1.000000000000000000 ) ) ;
#26274 = EDGE_CURVE ( 'NONE', #18076, #18272, #6723, .T. ) ;
#26275 = CIRCLE ( 'NONE', #9782, 55.86582179324592090 ) ;
#26276 = CARTESIAN_POINT ( 'NONE',  ( 158.0000000000011369, 98.11412463215494029, 45.00000000000000000 ) ) ;
#26277 = CARTESIAN_POINT ( 'NONE',  ( 158.0000000000001705, 190.9054999099155054, 45.00000000000000000 ) ) ;
#26278 = AXIS2_PLACEMENT_3D ( 'NONE', #1244, #7717, #25096 ) ;
#26279 = ADVANCED_FACE ( 'NONE', ( #24184 ), #19864, .T. ) ;
#26280 = CARTESIAN_POINT ( 'NONE',  ( -38.15920525445427103, 129.9964506885557967, 15.32335565452434523 ) ) ;
#26281 = EDGE_CURVE ( 'NONE', #4081, #14018, #23340, .T. ) ;
#26282 = DIRECTION ( 'NONE',  ( -0.000000000000000000, 1.000000000000000000, -1.387778780781445429E-16 ) ) ;
#26283 = CARTESIAN_POINT ( 'NONE',  ( -169.4960802787495027, 115.4387886157293650, 26.69851561402025197 ) ) ;
#26284 = CARTESIAN_POINT ( 'NONE',  ( -260.0000000000001137, -170.0000000000001137, 60.00000000000002132 ) ) ;
#26286 = ORIENTED_EDGE ( 'NONE', *, *, #8000, .F. ) ;
#26285 = ORIENTED_EDGE ( 'NONE', *, *, #22353, .T. ) ;
#26287 = CARTESIAN_POINT ( 'NONE',  ( 372.9108539694884144, 44.41075299063184190, 74.80456309157131045 ) ) ;
#26288 = CARTESIAN_POINT ( 'NONE',  ( -270.1025481742786951, -91.18033988749901653, 0.000000000000000000 ) ) ;
#26289 = ORIENTED_EDGE ( 'NONE', *, *, #15765, .T. ) ;
#26290 = ORIENTED_EDGE ( 'NONE', *, *, #15298, .T. ) ;
#26291 = CIRCLE ( 'NONE', #13936, 5.999999999999991118 ) ;
#26292 = EDGE_LOOP ( 'NONE', ( #6755, #10670, #27943, #5031 ) ) ;
#26293 = DIRECTION ( 'NONE',  ( 0.8916010070293783896, -0.4528218681382319422, 0.000000000000000000 ) ) ;
#26294 = LINE ( 'NONE', #13239, #21848 ) ;
#26295 = VERTEX_POINT ( 'NONE', #23900 ) ;
#26296 = VECTOR ( 'NONE', #1688, 1000.000000000000000 ) ;
#26297 = CARTESIAN_POINT ( 'NONE',  ( 104.4199312700659448, 89.58810137561040676, -100.0000000000000142 ) ) ;
#26298 = CARTESIAN_POINT ( 'NONE',  ( 157.9999999999996874, 266.6496251426330559, -45.00000000000000000 ) ) ;
#26299 = ORIENTED_EDGE ( 'NONE', *, *, #8328, .F. ) ;
#26300 = CARTESIAN_POINT ( 'NONE',  ( -214.3655805135422838, 87.98073541835873357, 21.65873204582219813 ) ) ;
#26301 = CARTESIAN_POINT ( 'NONE',  ( 157.9999999999998010, 241.0630000600560550, -45.00000000000000000 ) ) ;
#26302 = CARTESIAN_POINT ( 'NONE',  ( 158.0000000000016200, 52.97237449702815582, 45.00000000000000000 ) ) ;
#26303 = CARTESIAN_POINT ( 'NONE',  ( 158.2674871941218839, 201.0613226313178075, -148.6640466283485580 ) ) ;
#26304 = VECTOR ( 'NONE', #13679, 1000.000000000000000 ) ;
#26305 = EDGE_CURVE ( 'NONE', #24450, #17486, #10689, .T. ) ;
#26306 = VERTEX_POINT ( 'NONE', #21746 ) ;
#26307 = CIRCLE ( 'NONE', #26769, 5.999999999999977796 ) ;
#26308 = LINE ( 'NONE', #6635, #8667 ) ;
#26309 = EDGE_CURVE ( 'NONE', #548, #7521, #19446, .T. ) ;
#26310 = DIRECTION ( 'NONE',  ( -0.000000000000000000, 0.000000000000000000, -1.000000000000000000 ) ) ;
#26311 = DIRECTION ( 'NONE',  ( 0.000000000000000000, -1.000000000000000000, 0.000000000000000000 ) ) ;
#26312 = VECTOR ( 'NONE', #17586, 1000.000000000000000 ) ;
#26313 = DIRECTION ( 'NONE',  ( -0.8916010070293995948, -0.4528218681381900867, 0.000000000000000000 ) ) ;
#26314 = ORIENTED_EDGE ( 'NONE', *, *, #15351, .F. ) ;
#26315 = CARTESIAN_POINT ( 'NONE',  ( -211.1960507716717643, -220.0000000000000568, -108.0220471272657363 ) ) ;
#26316 = CYLINDRICAL_SURFACE ( 'NONE', #22172, 30.00000000000000000 ) ;
#26317 = CARTESIAN_POINT ( 'NONE',  ( 330.9869376377542949, 44.41075299063183479, 288.0938197134494203 ) ) ;
#26318 = EDGE_LOOP ( 'NONE', ( #15562, #17001, #16738, #24849 ) ) ;
#26319 =( NAMED_UNIT ( * ) PLANE_ANGLE_UNIT ( ) SI_UNIT ( $, .RADIAN. ) );
#26320 = ORIENTED_EDGE ( 'NONE', *, *, #8742, .T. ) ;
#26321 = CYLINDRICAL_SURFACE ( 'NONE', #26680, 6.000000000000005329 ) ;
#26322 = CARTESIAN_POINT ( 'NONE',  ( -192.2760768220978491, 101.7456562315031050, -32.00549636916782958 ) ) ;
#26323 = ORIENTED_EDGE ( 'NONE', *, *, #22671, .F. ) ;
#26324 = ORIENTED_EDGE ( 'NONE', *, *, #16083, .T. ) ;
#26325 = CARTESIAN_POINT ( 'NONE',  ( -114.8320768295896670, 71.54464929955101127, 82.80879831960035631 ) ) ;
#26326 = DIRECTION ( 'NONE',  ( 0.5457381880580733924, 0.8379557447115514313, 0.000000000000000000 ) ) ;
#26328 = ADVANCED_FACE ( 'NONE', ( #2054 ), #13413, .F. ) ;
#26327 = ORIENTED_EDGE ( 'NONE', *, *, #1975, .F. ) ;
#26329 = ORIENTED_EDGE ( 'NONE', *, *, #17974, .F. ) ;
#26330 = VECTOR ( 'NONE', #19286, 1000.000000000000000 ) ;
#26331 = DIRECTION ( 'NONE',  ( 0.000000000000000000, 0.000000000000000000, -1.000000000000000000 ) ) ;
#26332 = ADVANCED_FACE ( 'NONE', ( #8806 ), #4914, .T. ) ;
#26333 = DIRECTION ( 'NONE',  ( 0.000000000000000000, -0.000000000000000000, -1.000000000000000000 ) ) ;
#26334 = CARTESIAN_POINT ( 'NONE',  ( -217.2892621185082760, 109.4029876883478352, 12.99999999999999822 ) ) ;
#26335 = DIRECTION ( 'NONE',  ( -1.000000000000000000, 0.000000000000000000, 0.000000000000000000 ) ) ;
#26336 = PLANE ( 'NONE',  #4044 ) ;
#26337 = LINE ( 'NONE', #15305, #12882 ) ;
#26338 = DIRECTION ( 'NONE',  ( 0.000000000000000000, 0.000000000000000000, 1.000000000000000000 ) ) ;
#26339 = ORIENTED_EDGE ( 'NONE', *, *, #15960, .T. ) ;
#26340 = PLANE ( 'NONE',  #6261 ) ;
#26341 = EDGE_CURVE ( 'NONE', #20107, #8966, #22599, .T. ) ;
#26342 = DIRECTION ( 'NONE',  ( 1.000000000000000000, -1.902611372570518757E-15, 0.000000000000000000 ) ) ;
#26343 = CARTESIAN_POINT ( 'NONE',  ( 157.9999999999998579, 219.0000000000000284, 45.00000000000000000 ) ) ;
#26344 = ORIENTED_EDGE ( 'NONE', *, *, #3413, .T. ) ;
#26345 = CARTESIAN_POINT ( 'NONE',  ( 157.9999999999997158, 263.6338751276190351, 45.00000000000000000 ) ) ;
#26346 = ORIENTED_EDGE ( 'NONE', *, *, #19088, .F. ) ;
#26347 = EDGE_CURVE ( 'NONE', #28117, #8556, #5347, .T. ) ;
#26348 = DIRECTION ( 'NONE',  ( 0.2588190451025122463, -0.9659258262890706437, 0.000000000000000000 ) ) ;
#26349 = CARTESIAN_POINT ( 'NONE',  ( -270.0172489267828269, -165.2082603419176223, 88.28568317613442673 ) ) ;
#26350 = PLANE ( 'NONE',  #20889 ) ;
#26351 = CARTESIAN_POINT ( 'NONE',  ( 48.74042075079900371, -13.05995637893015449, 45.00000000000000000 ) ) ;
#26352 = SURFACE_SIDE_STYLE ('',( #22050 ) ) ;
#26353 = VECTOR ( 'NONE', #959, 1000.000000000000000 ) ;
#26354 = ORIENTED_EDGE ( 'NONE', *, *, #23476, .T. ) ;
#26355 = CARTESIAN_POINT ( 'NONE',  ( -221.2437346188302172, 71.40151075288129334, 20.77520232899931685 ) ) ;
#26356 = VERTEX_POINT ( 'NONE', #898 ) ;
#26357 = CARTESIAN_POINT ( 'NONE',  ( -263.9606520309740176, -171.3050423792260801, 94.90504062136166397 ) ) ;
#26358 = ORIENTED_EDGE ( 'NONE', *, *, #14843, .T. ) ;
#26359 = ADVANCED_FACE ( 'NONE', ( #16282 ), #12263, .T. ) ;
#26360 = ORIENTED_EDGE ( 'NONE', *, *, #12, .T. ) ;
#26361 = CARTESIAN_POINT ( 'NONE',  ( 114.5814157129578916, 209.3660254037841923, 45.00000000000000000 ) ) ;
#26362 = ORIENTED_EDGE ( 'NONE', *, *, #23533, .T. ) ;
#26363 = ORIENTED_EDGE ( 'NONE', *, *, #19261, .T. ) ;
#26364 = CARTESIAN_POINT ( 'NONE',  ( -217.7546030100696157, 138.5587306369054659, 15.07876772300363477 ) ) ;
#26365 = AXIS2_PLACEMENT_3D ( 'NONE', #13360, #13082, #22109 ) ;
#26366 = CARTESIAN_POINT ( 'NONE',  ( 91.66503723322182395, 240.0531355366313448, 6.981029948440133914 ) ) ;
#26367 = ADVANCED_FACE ( 'NONE', ( #13848 ), #9951, .T. ) ;
#26368 = DIRECTION ( 'NONE',  ( 0.2066290158914672603, 0.9784193629480785193, -0.000000000000000000 ) ) ;
#26369 = FACE_OUTER_BOUND ( 'NONE', #8430, .T. ) ;
#26370 = VECTOR ( 'NONE', #23605, 1000.000000000000114 ) ;
#26371 = CARTESIAN_POINT ( 'NONE',  ( 157.4999999999998579, 173.6043123611196961, -45.00000000000000000 ) ) ;
#26372 = LINE ( 'NONE', #6420, #23627 ) ;
#26373 = CARTESIAN_POINT ( 'NONE',  ( 2.016757918737204225, -1.249999999999998890, -7.548718989644206623 ) ) ;
#26374 = CARTESIAN_POINT ( 'NONE',  ( 89.99999999999994316, -70.00000000000001421, -25.00000000000000711 ) ) ;
#26375 = DIRECTION ( 'NONE',  ( 0.000000000000000000, 0.000000000000000000, 1.000000000000000000 ) ) ;
#26376 = DIRECTION ( 'NONE',  ( 0.000000000000000000, -1.000000000000000000, 0.000000000000000000 ) ) ;
#26377 = DIRECTION ( 'NONE',  ( -0.000000000000000000, -0.000000000000000000, -1.000000000000000000 ) ) ;
#26378 = ORIENTED_EDGE ( 'NONE', *, *, #14530, .T. ) ;
#26379 = LINE ( 'NONE', #4270, #22060 ) ;
#26380 = ADVANCED_FACE ( 'NONE', ( #13704 ), #15919, .T. ) ;
#26381 = LINE ( 'NONE', #6709, #19451 ) ;
#26382 = VECTOR ( 'NONE', #6451, 1000.000000000000000 ) ;
#26383 = LINE ( 'NONE', #26825, #17498 ) ;
#26384 = ORIENTED_EDGE ( 'NONE', *, *, #3709, .F. ) ;
#26385 = AXIS2_PLACEMENT_3D ( 'NONE', #5115, #13759, #22510 ) ;
#26386 = DIRECTION ( 'NONE',  ( -0.8916010070294402290, -0.4528218681381102062, 0.000000000000000000 ) ) ;
#26387 = VERTEX_POINT ( 'NONE', #15863 ) ;
#26388 = CARTESIAN_POINT ( 'NONE',  ( -24.84958620104691818, 129.2502933934031262, -15.64834371897906173 ) ) ;
#26389 = VERTEX_POINT ( 'NONE', #7229 ) ;
#26390 = AXIS2_PLACEMENT_3D ( 'NONE', #706, #2412, #7169 ) ;
#26391 = VECTOR ( 'NONE', #5756, 1000.000000000000000 ) ;
#26392 = ADVANCED_FACE ( 'NONE', ( #7371 ), #16001, .F. ) ;
#26393 = ORIENTED_EDGE ( 'NONE', *, *, #4470, .T. ) ;
#26394 = ORIENTED_EDGE ( 'NONE', *, *, #6300, .T. ) ;
#26395 = ORIENTED_EDGE ( 'NONE', *, *, #9850, .T. ) ;
#26396 = ORIENTED_EDGE ( 'NONE', *, *, #546, .T. ) ;
#26397 = DIRECTION ( 'NONE',  ( -0.000000000000000000, -0.000000000000000000, -1.000000000000000000 ) ) ;
#26398 = EDGE_CURVE ( 'NONE', #24882, #26528, #11695, .T. ) ;
#26399 = DIRECTION ( 'NONE',  ( -0.000000000000000000, 1.000000000000000000, -1.387778780781445429E-16 ) ) ;
#26400 = VECTOR ( 'NONE', #14623, 1000.000000000000000 ) ;
#26401 = EDGE_CURVE ( 'NONE', #21920, #14507, #20437, .T. ) ;
#26402 = UNCERTAINTY_MEASURE_WITH_UNIT (LENGTH_MEASURE( 1.000000000000000082E-05 ), #26034, 'distance_accuracy_value', 'NONE');
#26403 = VECTOR ( 'NONE', #11256, 1000.000000000000000 ) ;
#26404 = FACE_OUTER_BOUND ( 'NONE', #16388, .T. ) ;
#26405 = CARTESIAN_POINT ( 'NONE',  ( -214.2313421016903021, 58.42887478691795167, 32.84133050938623910 ) ) ;
#26406 = LINE ( 'NONE', #28131, #25700 ) ;
#26407 = DIRECTION ( 'NONE',  ( 0.4528218681371722343, 0.8916010070299166257, -0.000000000000000000 ) ) ;
#26408 = CARTESIAN_POINT ( 'NONE',  ( -76.25760768171835480, 221.6666220619077876, 12.99999999999999822 ) ) ;
#26409 = CARTESIAN_POINT ( 'NONE',  ( 157.9999999999998295, 226.5236250225210313, -45.00000000000000000 ) ) ;
#26410 = VECTOR ( 'NONE', #8543, 1000.000000000000000 ) ;
#26411 = FACE_OUTER_BOUND ( 'NONE', #15417, .T. ) ;
#26412 = LINE ( 'NONE', #10628, #7004 ) ;
#26413 = CARTESIAN_POINT ( 'NONE',  ( 157.4999999999998579, 118.4310621959647563, 45.00000000000000000 ) ) ;
#26414 = CARTESIAN_POINT ( 'NONE',  ( -208.6312261275415665, 71.65289352654478705, 39.58303953460989533 ) ) ;
#26415 = CARTESIAN_POINT ( 'NONE',  ( 187.4999999999996305, 83.06687458711267880, -42.86484227207692754 ) ) ;
#26416 = DIRECTION ( 'NONE',  ( 0.000000000000000000, -1.000000000000000000, 0.000000000000000000 ) ) ;
#26418 = EDGE_LOOP ( 'NONE', ( #9280, #11483, #12773, #10078 ) ) ;
#26417 = ORIENTED_EDGE ( 'NONE', *, *, #26881, .F. ) ;
#26419 = CARTESIAN_POINT ( 'NONE',  ( -169.3459405269803995, 115.5129628772605201, 26.63562761174981119 ) ) ;
#26420 = FACE_OUTER_BOUND ( 'NONE', #10072, .T. ) ;
#26421 = VERTEX_POINT ( 'NONE', #22311 ) ;
#26422 = ORIENTED_EDGE ( 'NONE', *, *, #3536, .T. ) ;
#26423 = VECTOR ( 'NONE', #19120, 1000.000000000000114 ) ;
#26424 = EDGE_LOOP ( 'NONE', ( #6321, #2577, #21700, #16963 ) ) ;
#26425 = CARTESIAN_POINT ( 'NONE',  ( -216.6285223362424119, 139.2238150404710382, -13.00000000000000000 ) ) ;
#26426 = CARTESIAN_POINT ( 'NONE',  ( -160.5161435040798494, 120.3804527765386609, 22.28951900308576128 ) ) ;
#26427 = ORIENTED_EDGE ( 'NONE', *, *, #6752, .T. ) ;
#26428 = AXIS2_PLACEMENT_3D ( 'NONE', #26200, #21611, #24062 ) ;
#26429 = ADVANCED_FACE ( 'NONE', ( #336 ), #18287, .T. ) ;
#26430 = CARTESIAN_POINT ( 'NONE',  ( 119.7545560452836639, 132.4900181920934870, -100.0000000000000142 ) ) ;
#26431 = EDGE_CURVE ( 'NONE', #17375, #27481, #25035, .T. ) ;
#26432 = CYLINDRICAL_SURFACE ( 'NONE', #17405, 22.49999999999999289 ) ;
#26433 = ORIENTED_EDGE ( 'NONE', *, *, #18399, .T. ) ;
#26434 = CARTESIAN_POINT ( 'NONE',  ( -212.5539796181134591, 88.28323935596885974, 22.89445012289458603 ) ) ;
#26435 = DIRECTION ( 'NONE',  ( 0.000000000000000000, -1.000000000000000000, 0.000000000000000000 ) ) ;
#26436 = PLANE ( 'NONE',  #7566 ) ;
#26437 = CARTESIAN_POINT ( 'NONE',  ( 158.9573448901061852, 201.9403141824000443, -140.2307156351394610 ) ) ;
#26438 = AXIS2_PLACEMENT_3D ( 'NONE', #15903, #5383, #9279 ) ;
#26439 = ORIENTED_EDGE ( 'NONE', *, *, #18193, .T. ) ;
#26440 = DIRECTION ( 'NONE',  ( 0.4528218681374120425, 0.8916010070297948342, -0.000000000000000000 ) ) ;
#26441 = CARTESIAN_POINT ( 'NONE',  ( -218.8273392347107631, 140.3457761587572747, -14.99191580167153681 ) ) ;
#26442 = CARTESIAN_POINT ( 'NONE',  ( 158.0000000000011084, 100.6219996396619791, 45.00000000000000000 ) ) ;
#26443 = DIRECTION ( 'NONE',  ( 0.3102637045530588500, -0.9506505318133536830, 0.000000000000000000 ) ) ;
#26444 = ORIENTED_EDGE ( 'NONE', *, *, #3475, .T. ) ;
#26445 = CARTESIAN_POINT ( 'NONE',  ( 187.4999999999996305, 494.4107529906318632, -74.99999999999995737 ) ) ;
#26446 = EDGE_CURVE ( 'NONE', #24140, #3327, #22874, .T. ) ;
#26447 = CARTESIAN_POINT ( 'NONE',  ( -160.8326600028555902, 120.2355194873575073, 21.37420696376536711 ) ) ;
#26448 = CARTESIAN_POINT ( 'NONE',  ( 432.4999999999996589, 19.41075299063184900, 87.99671038392668265 ) ) ;
#26449 = ORIENTED_EDGE ( 'NONE', *, *, #25377, .F. ) ;
#26450 = ORIENTED_EDGE ( 'NONE', *, *, #4531, .F. ) ;
#26451 = DIRECTION ( 'NONE',  ( -0.000000000000000000, -0.000000000000000000, -1.000000000000000000 ) ) ;
#26452 = CARTESIAN_POINT ( 'NONE',  ( -196.6099257382077496, 98.46903227932085656, -31.30702426071320943 ) ) ;
#26453 = ORIENTED_EDGE ( 'NONE', *, *, #8348, .F. ) ;
#26454 = EDGE_CURVE ( 'NONE', #11803, #8966, #2617, .T. ) ;
#26455 = AXIS2_PLACEMENT_3D ( 'NONE', #24466, #2762, #4773 ) ;
#26456 = ORIENTED_EDGE ( 'NONE', *, *, #6112, .F. ) ;
#26457 = EDGE_CURVE ( 'NONE', #5949, #24079, #9239, .T. ) ;
#26458 = CARTESIAN_POINT ( 'NONE',  ( 157.4999999999998579, 146.0176872785422404, -45.00000000000000000 ) ) ;
#26459 = ADVANCED_FACE ( 'NONE', ( #3182 ), #26607, .F. ) ;
#26460 = DIRECTION ( 'NONE',  ( 0.000000000000000000, 1.000000000000000000, 0.000000000000000000 ) ) ;
#26461 = EDGE_CURVE ( 'NONE', #3815, #28048, #12286, .T. ) ;
#26462 = VERTEX_POINT ( 'NONE', #16832 ) ;
#26463 = EDGE_LOOP ( 'NONE', ( #14181, #18632, #27576, #25444 ) ) ;
#26464 = CARTESIAN_POINT ( 'NONE',  ( 157.4999999999998579, 108.3995621659365867, -45.00000000000000000 ) ) ;
#26465 = DIRECTION ( 'NONE',  ( -0.000000000000000000, -0.000000000000000000, -1.000000000000000000 ) ) ;
#26466 = DIRECTION ( 'NONE',  ( -0.8916010070298563406, -0.4528218681372909171, 0.000000000000000000 ) ) ;
#26467 = CARTESIAN_POINT ( 'NONE',  ( 130.0130877889309602, 242.4751130497508029, 45.00000000000000000 ) ) ;
#26468 = LINE ( 'NONE', #6799, #5430 ) ;
#26469 = CARTESIAN_POINT ( 'NONE',  ( -209.0137638338787269, 69.92154464606612407, -37.51858872986124283 ) ) ;
#26470 = LINE ( 'NONE', #24059, #24742 ) ;
#26471 = VERTEX_POINT ( 'NONE', #27866 ) ;
#26472 = DIRECTION ( 'NONE',  ( 0.000000000000000000, 0.000000000000000000, 1.000000000000000000 ) ) ;
#26473 = DIRECTION ( 'NONE',  ( -0.000000000000000000, -0.000000000000000000, -1.000000000000000000 ) ) ;
#26474 = CYLINDRICAL_SURFACE ( 'NONE', #25173, 89.71075545852266941 ) ;
#26475 = CARTESIAN_POINT ( 'NONE',  ( 65.00000000000000000, -120.0000000000000711, 63.97500000000001563 ) ) ;
#26476 = CIRCLE ( 'NONE', #19627, 5.000000000000004441 ) ;
#26477 = EDGE_LOOP ( 'NONE', ( #27633, #13736, #17526, #1979 ) ) ;
#26478 = CARTESIAN_POINT ( 'NONE',  ( -225.0350560533458690, 62.39407306348317661, 8.837833373942171278 ) ) ;
#26479 = ORIENTED_EDGE ( 'NONE', *, *, #5266, .F. ) ;
#26480 = CARTESIAN_POINT ( 'NONE',  ( 117.5127944162877753, 203.5381304684075019, -45.00000000000000000 ) ) ;
#26481 = FACE_OUTER_BOUND ( 'NONE', #6828, .T. ) ;
#26482 = CARTESIAN_POINT ( 'NONE',  ( 140.8457514438942155, 249.4249679671852107, -146.3660979730027520 ) ) ;
#26483 = ORIENTED_EDGE ( 'NONE', *, *, #6497, .T. ) ;
#26484 = FACE_OUTER_BOUND ( 'NONE', #8288, .T. ) ;
#26485 =( LENGTH_UNIT ( ) NAMED_UNIT ( * ) SI_UNIT ( .MILLI., .METRE. ) );
#26486 = ORIENTED_EDGE ( 'NONE', *, *, #15315, .T. ) ;
#26487 = EDGE_CURVE ( 'NONE', #2726, #1215, #20992, .T. ) ;
#26488 = ADVANCED_FACE ( 'NONE', ( #27730 ), #25447, .F. ) ;
#26489 = LINE ( 'NONE', #24346, #7926 ) ;
#26490 = ORIENTED_EDGE ( 'NONE', *, *, #15463, .F. ) ;
#26491 = CARTESIAN_POINT ( 'NONE',  ( -276.0611529335072305, -165.0000000000001137, 107.4663680683487001 ) ) ;
#26492 = VERTEX_POINT ( 'NONE', #8069 ) ;
#26493 = EDGE_LOOP ( 'NONE', ( #7158, #27201, #23112, #5092 ) ) ;
#26494 = PLANE ( 'NONE',  #4406 ) ;
#26495 = VERTEX_POINT ( 'NONE', #3466 ) ;
#26496 = TOROIDAL_SURFACE ( 'NONE', #1727, 34.99999999999999289, 5.000000000000000000 ) ;
#26497 = EDGE_CURVE ( 'NONE', #4389, #11934, #18840, .T. ) ;
#26498 = CIRCLE ( 'NONE', #20562, 6.000000000000005329 ) ;
#26499 = ORIENTED_EDGE ( 'NONE', *, *, #13609, .F. ) ;
#26500 = ORIENTED_EDGE ( 'NONE', *, *, #18595, .F. ) ;
#26501 = DIRECTION ( 'NONE',  ( 1.000000000000000000, -0.000000000000000000, -0.000000000000000000 ) ) ;
#26502 = CARTESIAN_POINT ( 'NONE',  ( 93.26488863017658559, 240.2518291191169340, 7.855680688306072135 ) ) ;
#26503 = EDGE_CURVE ( 'NONE', #1515, #23197, #18226, .T. ) ;
#26504 = CARTESIAN_POINT ( 'NONE',  ( 199.9999999999998863, -150.0000000000000284, 110.0000000000000284 ) ) ;
#26505 = LINE ( 'NONE', #2376, #11010 ) ;
#26506 = DIRECTION ( 'NONE',  ( -0.000000000000000000, -0.000000000000000000, -1.000000000000000000 ) ) ;
#26507 = DIRECTION ( 'NONE',  ( 4.540956701092242152E-16, 1.000000000000000000, 0.000000000000000000 ) ) ;
#26508 = CARTESIAN_POINT ( 'NONE',  ( 157.9999999999997726, 246.0787500750700474, 45.00000000000000000 ) ) ;
#26509 = PRESENTATION_LAYER_ASSIGNMENT (  '', '', ( #19179 ) ) ;
#26510 = SPHERICAL_SURFACE ( 'NONE', #18195, 5.000000000000000000 ) ;
#26511 = DIRECTION ( 'NONE',  ( 1.000000000000000000, 0.000000000000000000, 0.000000000000000000 ) ) ;
#26512 = DIRECTION ( 'NONE',  ( -0.8916010070297244461, -0.4528218681375507093, 0.000000000000000000 ) ) ;
#26513 = CARTESIAN_POINT ( 'NONE',  ( -143.6428522700808230, 71.54464929955099706, 83.00000000000001421 ) ) ;
#26514 = DIRECTION ( 'NONE',  ( 0.6533458216954761699, -0.7570595995514904919, 0.000000000000000000 ) ) ;
#26515 = ORIENTED_EDGE ( 'NONE', *, *, #15464, .F. ) ;
#26516 = PLANE ( 'NONE',  #11524 ) ;
#26517 = VECTOR ( 'NONE', #21653, 1000.000000000000000 ) ;
#26518 = VECTOR ( 'NONE', #2558, 1000.000000000000000 ) ;
#26519 = CARTESIAN_POINT ( 'NONE',  ( 157.9999999999997442, 249.0945000900840398, 45.00000000000000000 ) ) ;
#26520 = FACE_OUTER_BOUND ( 'NONE', #3790, .T. ) ;
#26521 = CARTESIAN_POINT ( 'NONE',  ( 107.7914849032574551, 207.3616777871659167, -139.6178255645964441 ) ) ;
#26522 = ORIENTED_EDGE ( 'NONE', *, *, #23941, .T. ) ;
#26523 = EDGE_CURVE ( 'NONE', #25624, #1908, #9807, .T. ) ;
#26524 = ADVANCED_FACE ( 'NONE', ( #23012 ), #18984, .F. ) ;
#26525 = CARTESIAN_POINT ( 'NONE',  ( 108.2753065237224774, 248.3531133182295321, -34.86527342668098584 ) ) ;
#26526 = ORIENTED_EDGE ( 'NONE', *, *, #9732, .F. ) ;
#26527 = CARTESIAN_POINT ( 'NONE',  ( 134.9999999999998579, 220.0000000000000284, 90.00000000000002842 ) ) ;
#26528 = VERTEX_POINT ( 'NONE', #1597 ) ;
#26529 = EDGE_LOOP ( 'NONE', ( #17351, #17886, #6102, #2181 ) ) ;
#26530 = AXIS2_PLACEMENT_3D ( 'NONE', #717, #18239, #15025 ) ;
#26531 = ORIENTED_EDGE ( 'NONE', *, *, #11493, .T. ) ;
#26532 = ORIENTED_EDGE ( 'NONE', *, *, #12389, .F. ) ;
#26533 = ORIENTED_EDGE ( 'NONE', *, *, #12174, .F. ) ;
#26534 = ORIENTED_EDGE ( 'NONE', *, *, #13688, .T. ) ;
#26535 = CARTESIAN_POINT ( 'NONE',  ( 134.9999999999998579, 220.0000000000000284, 99.00000000000001421 ) ) ;
#26536 = CARTESIAN_POINT ( 'NONE',  ( 222.4999999999996021, 186.4134324495536248, 35.02193266779035952 ) ) ;
#26537 = AXIS2_PLACEMENT_3D ( 'NONE', #17165, #25923, #23773 ) ;
#26538 = EDGE_CURVE ( 'NONE', #1356, #12421, #5904, .T. ) ;
#26539 = ADVANCED_FACE ( 'NONE', ( #23434 ), #23296, .F. ) ;
#26540 = CIRCLE ( 'NONE', #13255, 30.00000000000000000 ) ;
#26541 = FACE_OUTER_BOUND ( 'NONE', #22731, .T. ) ;
#26542 = CARTESIAN_POINT ( 'NONE',  ( 187.4999999999996305, 133.0668745871126930, -42.86484227207692044 ) ) ;
#26543 = AXIS2_PLACEMENT_3D ( 'NONE', #28159, #12400, #8499 ) ;
#26544 = CARTESIAN_POINT ( 'NONE',  ( -226.6532499065066020, 62.99057865342218321, 8.245540320826911795 ) ) ;
#26545 = PLANE ( 'NONE',  #22738 ) ;
#26546 = DIRECTION ( 'NONE',  ( 0.4528218681383106015, -0.8916010070293384215, 0.000000000000000000 ) ) ;
#26547 = DIRECTION ( 'NONE',  ( 1.000000000000000000, 0.000000000000000000, -0.000000000000000000 ) ) ;
#26548 = LINE ( 'NONE', #6880, #14014 ) ;
#26549 = LINE ( 'NONE', #2995, #11390 ) ;
#26550 = CARTESIAN_POINT ( 'NONE',  ( 101.7779539749746931, 119.2876405404125393, 82.50000000030260594 ) ) ;
#26551 = EDGE_CURVE ( 'NONE', #18428, #23530, #12114, .T. ) ;
#26552 = ADVANCED_FACE ( 'NONE', ( #3323 ), #10368, .F. ) ;
#26554 = CARTESIAN_POINT ( 'NONE',  ( 7.501147730487500276, 138.6545231272701528, 14.99999999999999467 ) ) ;
#26553 = CIRCLE ( 'NONE', #17848, 10.00000000000000888 ) ;
#26555 = DIRECTION ( 'NONE',  ( -1.000000000000000000, 4.540956701092242152E-16, 0.000000000000000000 ) ) ;
#26556 = AXIS2_PLACEMENT_3D ( 'NONE', #4111, #12895, #4254 ) ;
#26557 = CARTESIAN_POINT ( 'NONE',  ( 184.9999999999999147, -150.0000000000000284, -84.99999999999997158 ) ) ;
#26558 = CARTESIAN_POINT ( 'NONE',  ( -28.05246235954390244, 188.0718642840173516, 12.99999999999999822 ) ) ;
#26560 = EDGE_LOOP ( 'NONE', ( #20697, #6889, #22489, #20979, #19762, #13634, #3502, #19233 ) ) ;
#26559 = ORIENTED_EDGE ( 'NONE', *, *, #18672, .T. ) ;
#26561 = FACE_OUTER_BOUND ( 'NONE', #44, .T. ) ;
#26562 = VECTOR ( 'NONE', #18240, 1000.000000000000114 ) ;
#26563 = DIRECTION ( 'NONE',  ( -0.000000000000000000, 0.000000000000000000, -1.000000000000000000 ) ) ;
#26564 = DIRECTION ( 'NONE',  ( 0.000000000000000000, 0.000000000000000000, -1.000000000000000000 ) ) ;
#26565 = ORIENTED_EDGE ( 'NONE', *, *, #13132, .F. ) ;
#26566 = VERTEX_POINT ( 'NONE', #5629 ) ;
#26567 = AXIS2_PLACEMENT_3D ( 'NONE', #204, #8965, #4222 ) ;
#26569 = ORIENTED_EDGE ( 'NONE', *, *, #18603, .F. ) ;
#26568 = CONICAL_SURFACE ( 'NONE', #21530, 18.91107291867258411, 0.08885387018394237668 ) ;
#26570 = PLANE ( 'NONE',  #25340 ) ;
#26571 = CARTESIAN_POINT ( 'NONE',  ( -158.3304926817754676, 121.3760726389792666, 21.42757541440370872 ) ) ;
#26572 = ORIENTED_EDGE ( 'NONE', *, *, #18887, .T. ) ;
#26573 = EDGE_LOOP ( 'NONE', ( #8745, #23059, #26919, #11467 ) ) ;
#26574 = CARTESIAN_POINT ( 'NONE',  ( -42.53273978471831640, 130.9733465240572627, 14.93735646117640847 ) ) ;
#26575 = EDGE_CURVE ( 'NONE', #22496, #13270, #25725, .T. ) ;
#26576 = CARTESIAN_POINT ( 'NONE',  ( -41.54405845664282282, 46.26118624020713099, 45.00000000000000000 ) ) ;
#26577 = CIRCLE ( 'NONE', #10026, 14.64217782292691261 ) ;
#26578 = VERTEX_POINT ( 'NONE', #7653 ) ;
#26579 = CARTESIAN_POINT ( 'NONE',  ( 158.0000000000005969, 148.7794997898028271, 45.00000000000000000 ) ) ;
#26580 = CARTESIAN_POINT ( 'NONE',  ( 157.9999999999997158, 261.6338751276190351, 45.00000000000000000 ) ) ;
#26581 = AXIS2_PLACEMENT_3D ( 'NONE', #3099, #13624, #15922 ) ;
#26582 = CARTESIAN_POINT ( 'NONE',  ( 199.9999999999998863, -160.0000000000000853, 110.0000000000000284 ) ) ;
#26583 = CARTESIAN_POINT ( 'NONE',  ( 160.7828204114136952, 204.6609985789451969, -139.0095862629495116 ) ) ;
#26584 = CARTESIAN_POINT ( 'NONE',  ( -195.7913036700337841, 62.61587363931871408, -36.00381397819591456 ) ) ;
#26585 = VECTOR ( 'NONE', #92, 1000.000000000000114 ) ;
#26586 = VERTEX_POINT ( 'NONE', #16554 ) ;
#26587 = CARTESIAN_POINT ( 'NONE',  ( 158.0000000000016769, 45.95662448201407102, -45.00000000000000000 ) ) ;
#26588 = CARTESIAN_POINT ( 'NONE',  ( -223.0228900756071653, 134.9178336739567499, -12.97939780113087060 ) ) ;
#26589 = DIRECTION ( 'NONE',  ( -1.000000000000000000, 0.000000000000000000, 3.053113317719176147E-15 ) ) ;
#26590 = DIRECTION ( 'NONE',  ( 0.8379557447115514313, -0.5457381880580733924, 0.000000000000000000 ) ) ;
#26591 = VERTEX_POINT ( 'NONE', #14264 ) ;
#26592 = EDGE_CURVE ( 'NONE', #23775, #23149, #23581, .T. ) ;
#26593 = CARTESIAN_POINT ( 'NONE',  ( -175.8417606860892874, 246.9430296707336652, 12.99999999999999822 ) ) ;
#26594 = ADVANCED_FACE ( 'NONE', ( #1036 ), #20928, .F. ) ;
#26595 = AXIS2_PLACEMENT_3D ( 'NONE', #11158, #19911, #24361 ) ;
#26596 = DIRECTION ( 'NONE',  ( -0.8916010070295112833, -0.4528218681379702626, 0.000000000000000000 ) ) ;
#26597 = LINE ( 'NONE', #24746, #4366 ) ;
#26598 = ORIENTED_EDGE ( 'NONE', *, *, #25234, .T. ) ;
#26599 = EDGE_CURVE ( 'NONE', #13520, #15076, #12733, .T. ) ;
#26600 = ORIENTED_EDGE ( 'NONE', *, *, #18562, .T. ) ;
#26601 = AXIS2_PLACEMENT_3D ( 'NONE', #23604, #12841, #1622 ) ;
#26602 = CARTESIAN_POINT ( 'NONE',  ( -236.8177751472017007, 82.33896643611701904, 5.000000000000002665 ) ) ;
#26603 = DIRECTION ( 'NONE',  ( 1.000000000000000000, 0.000000000000000000, -0.000000000000000000 ) ) ;
#26604 = VECTOR ( 'NONE', #27009, 1000.000000000000000 ) ;
#26605 = ORIENTED_EDGE ( 'NONE', *, *, #5098, .T. ) ;
#26606 = ORIENTED_EDGE ( 'NONE', *, *, #7973, .F. ) ;
#26607 = PLANE ( 'NONE',  #26455 ) ;
#26608 = FACE_OUTER_BOUND ( 'NONE', #15905, .T. ) ;
#26609 = ORIENTED_EDGE ( 'NONE', *, *, #8389, .T. ) ;
#26610 = ORIENTED_EDGE ( 'NONE', *, *, #9225, .F. ) ;
#26611 = CARTESIAN_POINT ( 'NONE',  ( -266.5839533485339530, -91.18033988749901653, 0.000000000000000000 ) ) ;
#26612 = AXIS2_PLACEMENT_3D ( 'NONE', #21758, #26617, #2200 ) ;
#26613 = CARTESIAN_POINT ( 'NONE',  ( 338.9795809418241106, 102.2323340340494724, -145.0000000000000000 ) ) ;
#26614 = CARTESIAN_POINT ( 'NONE',  ( 157.4999999999995453, 206.2066874587088989, 45.00000000000000000 ) ) ;
#26615 = CARTESIAN_POINT ( 'NONE',  ( -7.828161053703414751, 131.1970564781817643, -16.31839186148043552 ) ) ;
#26616 = CARTESIAN_POINT ( 'NONE',  ( -175.0000000000000000, -170.0000000000001705, 76.00000000000000000 ) ) ;
#26617 = DIRECTION ( 'NONE',  ( 0.000000000000000000, 1.000000000000000000, -0.000000000000000000 ) ) ;
#26618 = VECTOR ( 'NONE', #27607, 1000.000000000000000 ) ;
#26619 = LINE ( 'NONE', #9108, #8061 ) ;
#26620 = ORIENTED_EDGE ( 'NONE', *, *, #8156, .F. ) ;
#26621 = DIRECTION ( 'NONE',  ( 0.8916010070296226386, 0.4528218681377511601, 0.000000000000000000 ) ) ;
#26622 = EDGE_CURVE ( 'NONE', #61, #1444, #15539, .T. ) ;
#26623 = LINE ( 'NONE', #8689, #14313 ) ;
#26624 = DIRECTION ( 'NONE',  ( -0.8916010070297244461, -0.4528218681375507093, 0.000000000000000000 ) ) ;
#26625 = DIRECTION ( 'NONE',  ( -1.000000000000000000, -0.000000000000000000, -0.000000000000000000 ) ) ;
#26626 = VERTEX_POINT ( 'NONE', #734 ) ;
#26627 = LINE ( 'NONE', #19608, #27034 ) ;
#26628 = EDGE_CURVE ( 'NONE', #15242, #1653, #24432, .T. ) ;
#26629 = ORIENTED_EDGE ( 'NONE', *, *, #2197, .T. ) ;
#26630 = EDGE_CURVE ( 'NONE', #14597, #25416, #9510, .T. ) ;
#26631 = CARTESIAN_POINT ( 'NONE',  ( -175.0000000000000000, -120.0000000000001847, -69.99999999999998579 ) ) ;
#26632 = FACE_OUTER_BOUND ( 'NONE', #26059, .T. ) ;
#26633 = CARTESIAN_POINT ( 'NONE',  ( 139.5211538318895066, 249.6587006023211188, -141.0358260266775687 ) ) ;
#26634 = ORIENTED_EDGE ( 'NONE', *, *, #13201, .F. ) ;
#26635 = CARTESIAN_POINT ( 'NONE',  ( 158.0000000000016769, 45.95662448201407102, 45.00000000000000000 ) ) ;
#26636 = VERTEX_POINT ( 'NONE', #11225 ) ;
#26637 = AXIS2_PLACEMENT_3D ( 'NONE', #9617, #13944, #7317 ) ;
#26638 = CARTESIAN_POINT ( 'NONE',  ( -222.0899288397881435, 71.52493653041949528, 20.17326427264749711 ) ) ;
#26639 = EDGE_LOOP ( 'NONE', ( #17995, #5208, #5706, #20369 ) ) ;
#26640 = DIRECTION ( 'NONE',  ( 0.000000000000000000, 0.000000000000000000, -1.000000000000000000 ) ) ;
#26641 = ORIENTED_EDGE ( 'NONE', *, *, #15621, .F. ) ;
#26642 = VERTEX_POINT ( 'NONE', #26574 ) ;
#26643 = CARTESIAN_POINT ( 'NONE',  ( 134.9999999999998579, 220.0000000000000284, 84.99999999999995737 ) ) ;
#26644 = ORIENTED_EDGE ( 'NONE', *, *, #5300, .T. ) ;
#26645 = CIRCLE ( 'NONE', #28023, 11.42311362948588105 ) ;
#26646 = ORIENTED_EDGE ( 'NONE', *, *, #27303, .T. ) ;
#26647 = ORIENTED_EDGE ( 'NONE', *, *, #1620, .T. ) ;
#26648 = CARTESIAN_POINT ( 'NONE',  ( 105.1668099567775414, 241.3986356328032628, 28.65150506303233513 ) ) ;
#26649 = CARTESIAN_POINT ( 'NONE',  ( 157.4999999999998579, 45.70268697826052318, 45.00000000000000000 ) ) ;
#26650 = PLANE ( 'NONE',  #6429 ) ;
#26651 = ADVANCED_FACE ( 'NONE', ( #11523 ), #19977, .F. ) ;
#26652 = LINE ( 'NONE', #26235, #14696 ) ;
#26653 = EDGE_CURVE ( 'NONE', #9022, #13594, #450, .T. ) ;
#26654 = CARTESIAN_POINT ( 'NONE',  ( 115.6411010564578561, 208.5333949360010308, 99.00000000000001421 ) ) ;
#26655 = DIRECTION ( 'NONE',  ( 0.4528218681383106015, -0.8916010070293384215, 0.000000000000000000 ) ) ;
#26656 = AXIS2_PLACEMENT_3D ( 'NONE', #7137, #11164, #26659 ) ;
#26657 = LINE ( 'NONE', #17475, #14078 ) ;
#26658 = DIRECTION ( 'NONE',  ( -0.000000000000000000, -1.000000000000000000, -0.000000000000000000 ) ) ;
#26659 = DIRECTION ( 'NONE',  ( -0.000000000000000000, 0.000000000000000000, -1.000000000000000000 ) ) ;
#26660 = CARTESIAN_POINT ( 'NONE',  ( 157.4999999999995453, 206.2066874587088989, 45.00000000000000000 ) ) ;
#26661 = CARTESIAN_POINT ( 'NONE',  ( 119.9999999999999147, 203.2294901687515676, 100.0000000000000142 ) ) ;
#26662 = ORIENTED_EDGE ( 'NONE', *, *, #26401, .T. ) ;
#26663 = PLANE ( 'NONE',  #27540 ) ;
#26664 = EDGE_CURVE ( 'NONE', #170, #24882, #17969, .T. ) ;
#26665 = VECTOR ( 'NONE', #13627, 1000.000000000000114 ) ;
#26666 = ADVANCED_FACE ( 'NONE', ( #20261 ), #9063, .F. ) ;
#26667 = DIRECTION ( 'NONE',  ( 1.000000000000000000, 0.000000000000000000, -0.000000000000000000 ) ) ;
#26668 = CARTESIAN_POINT ( 'NONE',  ( 158.0000000000015916, 55.48024950453520177, 45.00000000000000000 ) ) ;
#26669 = FACE_OUTER_BOUND ( 'NONE', #23600, .T. ) ;
#26670 = ORIENTED_EDGE ( 'NONE', *, *, #22462, .T. ) ;
#26671 = LINE ( 'NONE', #17636, #13924 ) ;
#26672 = ORIENTED_EDGE ( 'NONE', *, *, #8102, .T. ) ;
#26673 = PRESENTATION_STYLE_ASSIGNMENT (( #4983 ) ) ;
#26674 = EDGE_LOOP ( 'NONE', ( #10130, #25615, #19357, #12708, #24900, #16837, #434, #2014, #14057, #17428, #9690, #3670 ) ) ;
#26675 = ORIENTED_EDGE ( 'NONE', *, *, #16351, .T. ) ;
#26676 = VECTOR ( 'NONE', #4367, 1000.000000000000000 ) ;
#26677 = ORIENTED_EDGE ( 'NONE', *, *, #12799, .F. ) ;
#26678 = VERTEX_POINT ( 'NONE', #22712 ) ;
#26679 = VERTEX_POINT ( 'NONE', #3017 ) ;
#26680 = AXIS2_PLACEMENT_3D ( 'NONE', #13136, #2183, #24462 ) ;
#26681 = VERTEX_POINT ( 'NONE', #24862 ) ;
#26682 = VECTOR ( 'NONE', #18032, 1000.000000000000000 ) ;
#26683 = FACE_OUTER_BOUND ( 'NONE', #12782, .T. ) ;
#26684 = CARTESIAN_POINT ( 'NONE',  ( 158.0000000000000853, 198.4291249324366504, 45.00000000000000000 ) ) ;
#26685 = VECTOR ( 'NONE', #14602, 1000.000000000000000 ) ;
#26686 = CARTESIAN_POINT ( 'NONE',  ( 158.0000000000012506, 88.08262460212675649, 45.00000000000000000 ) ) ;
#26687 = ADVANCED_FACE ( 'NONE', ( #11805 ), #9502, .F. ) ;
#26688 = CARTESIAN_POINT ( 'NONE',  ( -310.0000000000001137, -157.0000000000000284, 60.00000000000002842 ) ) ;
#26689 = CARTESIAN_POINT ( 'NONE',  ( -221.7690971916811407, 71.47334710437667127, 20.39711061091035305 ) ) ;
#26690 = LINE ( 'NONE', #17940, #17361 ) ;
#26691 = ADVANCED_FACE ( 'NONE', ( #15683 ), #22131, .F. ) ;
#26692 = DIRECTION ( 'NONE',  ( -0.8916010070294098089, -0.4528218681381701027, 0.000000000000000000 ) ) ;
#26693 = CARTESIAN_POINT ( 'NONE',  ( 157.4999999999998579, 143.5098122710352015, -45.00000000000000000 ) ) ;
#26694 = CARTESIAN_POINT ( 'NONE',  ( 157.4999999999996305, 288.9665627064425735, 45.00000000000000000 ) ) ;
#26695 = FACE_OUTER_BOUND ( 'NONE', #16579, .T. ) ;
#26696 = DIRECTION ( 'NONE',  ( -0.000000000000000000, -0.000000000000000000, -1.000000000000000000 ) ) ;
#26697 = CARTESIAN_POINT ( 'NONE',  ( 2.399999999999999911, 1.249999999999999556, 8.000000000000000000 ) ) ;
#26698 = VECTOR ( 'NONE', #24448, 1000.000000000000000 ) ;
#26699 = CARTESIAN_POINT ( 'NONE',  ( 157.4999999999998579, 85.82868709837320864, -45.00000000000000000 ) ) ;
#26700 = EDGE_CURVE ( 'NONE', #19053, #969, #2588, .T. ) ;
#26701 = CARTESIAN_POINT ( 'NONE',  ( -210.0000000000000284, -3.238150488490040751E-14, 70.00000000000001421 ) ) ;
#26702 = LINE ( 'NONE', #22258, #4632 ) ;
#26703 = DIRECTION ( 'NONE',  ( -0.000000000000000000, -0.000000000000000000, -1.000000000000000000 ) ) ;
#26704 = VECTOR ( 'NONE', #15966, 1000.000000000000000 ) ;
#26706 = VERTEX_POINT ( 'NONE', #9641 ) ;
#26705 = EDGE_LOOP ( 'NONE', ( #11848, #20214, #2658, #22456 ) ) ;
#26707 = AXIS2_PLACEMENT_3D ( 'NONE', #16272, #18692, #14533 ) ;
#26708 = DIRECTION ( 'NONE',  ( 1.000000000000000000, 1.530283246943720875E-16, -0.000000000000000000 ) ) ;
#26709 = VECTOR ( 'NONE', #8526, 1000.000000000000000 ) ;
#26710 = EDGE_CURVE ( 'NONE', #9201, #194, #26723, .T. ) ;
#26711 = DIRECTION ( 'NONE',  ( 0.4528218681378317068, 0.8916010070295816714, -0.000000000000000000 ) ) ;
#26712 = CARTESIAN_POINT ( 'NONE',  ( -209.0165584120921096, 88.62137859748428070, -26.02317696115059320 ) ) ;
#26713 = ORIENTED_EDGE ( 'NONE', *, *, #21676, .F. ) ;
#26714 = ORIENTED_EDGE ( 'NONE', *, *, #17792, .T. ) ;
#26715 = ORIENTED_EDGE ( 'NONE', *, *, #15595, .T. ) ;
#26716 = CARTESIAN_POINT ( 'NONE',  ( 158.0000000000001421, 191.4133749174225443, 45.00000000000000000 ) ) ;
#26717 = CARTESIAN_POINT ( 'NONE',  ( -134.0236137306590365, 130.0100214678653003, 15.30004249603843469 ) ) ;
#26718 = ORIENTED_EDGE ( 'NONE', *, *, #24762, .T. ) ;
#26719 = ORIENTED_EDGE ( 'NONE', *, *, #17819, .F. ) ;
#26720 = B_SPLINE_CURVE_WITH_KNOTS ( 'NONE', 3,
 ( #24193, #2064, #22034, #15579, #26056, #6666, #17865, #28200 ),
 .UNSPECIFIED., .F., .F.,
 ( 4, 2, 2, 4 ),
 ( 0.000000000000000000, 0.004191298939714996341, 0.008382597879429992682, 0.01676519575885998536 ),
 .UNSPECIFIED. ) ;
#26721 = EDGE_CURVE ( 'NONE', #10524, #27001, #24578, .T. ) ;
#26722 = AXIS2_PLACEMENT_3D ( 'NONE', #9746, #23099, #25390 ) ;
#26723 = LINE ( 'NONE', #4886, #24656 ) ;
#26724 = AXIS2_PLACEMENT_3D ( 'NONE', #26631, #18028, #20175 ) ;
#26725 = CARTESIAN_POINT ( 'NONE',  ( 137.6105238444007455, 239.8288972274759203, -45.00000000000000000 ) ) ;
#26726 = VERTEX_POINT ( 'NONE', #22420 ) ;
#26727 = CARTESIAN_POINT ( 'NONE',  ( -205.5899716318703554, 91.23091416471392279, 28.02219806143363812 ) ) ;
#26728 = AXIS2_PLACEMENT_3D ( 'NONE', #23385, #16645, #25116 ) ;
#26729 = CIRCLE ( 'NONE', #6849, 9.999999999999982236 ) ;
#26730 = LINE ( 'NONE', #26301, #26766 ) ;
#26731 = AXIS2_PLACEMENT_3D ( 'NONE', #1208, #25896, #1350 ) ;
#26732 = EDGE_CURVE ( 'NONE', #5554, #23150, #15971, .T. ) ;
#26733 = DIRECTION ( 'NONE',  ( 0.000000000000000000, -1.000000000000000000, 0.000000000000000000 ) ) ;
#26734 = DIRECTION ( 'NONE',  ( 0.000000000000000000, 0.000000000000000000, 1.000000000000000000 ) ) ;
#26735 = CARTESIAN_POINT ( 'NONE',  ( -204.6417490964368540, 60.41478268044598110, -22.13567842568586030 ) ) ;
#26736 = ORIENTED_EDGE ( 'NONE', *, *, #3905, .T. ) ;
#26737 = PLANE ( 'NONE',  #3604 ) ;
#26738 = CARTESIAN_POINT ( 'NONE',  ( 32.36067977499786252, -40.00000000000003553, 100.0000000000000142 ) ) ;
#26739 = DIRECTION ( 'NONE',  ( -0.8916010070296732648, 0.4528218681376511845, 0.000000000000000000 ) ) ;
#26740 = DIRECTION ( 'NONE',  ( -0.8916010070298360235, -0.4528218681373308852, 0.000000000000000000 ) ) ;
#26741 = VERTEX_POINT ( 'NONE', #24722 ) ;
#26742 = CIRCLE ( 'NONE', #24003, 22.49999999999999289 ) ;
#26743 = CARTESIAN_POINT ( 'NONE',  ( 157.4999999999998579, 128.4625622259929401, 45.00000000000000000 ) ) ;
#26744 = ADVANCED_FACE ( 'NONE', ( #13818 ), #22569, .F. ) ;
#26745 = EDGE_CURVE ( 'NONE', #21631, #14873, #18397, .T. ) ;
#26746 = VECTOR ( 'NONE', #1203, 1000.000000000000000 ) ;
#26747 = CARTESIAN_POINT ( 'NONE',  ( 79.99999999999994316, 1.480297366166874546E-14, -45.00000000000000000 ) ) ;
#26748 = LINE ( 'NONE', #2318, #7113 ) ;
#26749 = ORIENTED_EDGE ( 'NONE', *, *, #23521, .F. ) ;
#26750 = CARTESIAN_POINT ( 'NONE',  ( 0.000000000000000000, 0.000000000000000000, 0.000000000000000000 ) ) ;
#26751 = AXIS2_PLACEMENT_3D ( 'NONE', #21049, #9584, #20771 ) ;
#26752 = ORIENTED_EDGE ( 'NONE', *, *, #5684, .T. ) ;
#26753 = VECTOR ( 'NONE', #19897, 1000.000000000000000 ) ;
#26754 = DIRECTION ( 'NONE',  ( -0.8916010070299882351, -0.4528218681370311249, 0.000000000000000000 ) ) ;
#26755 = CARTESIAN_POINT ( 'NONE',  ( -202.3850906029173018, 93.73590935844725891, -29.14524087624419124 ) ) ;
#26756 = ORIENTED_EDGE ( 'NONE', *, *, #25457, .F. ) ;
#26757 = VECTOR ( 'NONE', #11709, 1000.000000000000000 ) ;
#26759 = EDGE_CURVE ( 'NONE', #26495, #4081, #4595, .T. ) ;
#26758 = ORIENTED_EDGE ( 'NONE', *, *, #20723, .F. ) ;
#26760 = CARTESIAN_POINT ( 'NONE',  ( 0.000000000000000000, 0.000000000000000000, -7.475068018844455153 ) ) ;
#26761 = DIRECTION ( 'NONE',  ( -0.000000000000000000, -0.000000000000000000, -1.000000000000000000 ) ) ;
#26762 = ORIENTED_EDGE ( 'NONE', *, *, #25553, .T. ) ;
#26763 = LINE ( 'NONE', #20578, #25196 ) ;
#26764 = VERTEX_POINT ( 'NONE', #3150 ) ;
#26765 = ADVANCED_FACE ( 'NONE', ( #20967 ), #10875, .F. ) ;
#26766 = VECTOR ( 'NONE', #17826, 1000.000000000000000 ) ;
#26767 = FACE_OUTER_BOUND ( 'NONE', #4480, .T. ) ;
#26768 = EDGE_CURVE ( 'NONE', #19061, #11111, #5452, .T. ) ;
#26769 = AXIS2_PLACEMENT_3D ( 'NONE', #181, #24454, #4763 ) ;
#26770 = DIRECTION ( 'NONE',  ( -4.540956701092242152E-16, -1.000000000000000000, -0.000000000000000000 ) ) ;
#26771 = EDGE_CURVE ( 'NONE', #12526, #2977, #6742, .T. ) ;
#26772 = CARTESIAN_POINT ( 'NONE',  ( 157.9999999999998863, 218.4921249924925348, 45.00000000000000000 ) ) ;
#26773 = CARTESIAN_POINT ( 'NONE',  ( -3.523879052116754895, 132.7919533277021742, -15.87505980800028560 ) ) ;
#26774 = VECTOR ( 'NONE', #10284, 1000.000000000000114 ) ;
#26775 = CARTESIAN_POINT ( 'NONE',  ( 158.0000000000004263, 166.3346248423521274, -45.00000000000000000 ) ) ;
#26776 = CARTESIAN_POINT ( 'NONE',  ( -230.8916957670046486, 130.8330661503598833, 15.00000000000000000 ) ) ;
#26777 = LINE ( 'NONE', #11846, #13784 ) ;
#26778 = VERTEX_POINT ( 'NONE', #14374 ) ;
#26779 = CARTESIAN_POINT ( 'NONE',  ( -175.0000000000000000, -120.0000000000001705, 70.00000000000001421 ) ) ;
#26780 = CARTESIAN_POINT ( 'NONE',  ( -190.0000000000000284, -40.00000000000004974, 80.00000000000001421 ) ) ;
#26781 = CARTESIAN_POINT ( 'NONE',  ( 158.0000000000009948, 108.6534996696901345, 45.00000000000000000 ) ) ;
#26782 = CARTESIAN_POINT ( 'NONE',  ( 432.4999999999996589, 19.41075299063184900, 87.99671038392668265 ) ) ;
#26783 = ORIENTED_EDGE ( 'NONE', *, *, #19889, .F. ) ;
#26784 = CARTESIAN_POINT ( 'NONE',  ( -160.0000000000000284, 79.99999999999994316, 100.0000000000000142 ) ) ;
#26785 = ORIENTED_EDGE ( 'NONE', *, *, #7994, .T. ) ;
#26786 = LINE ( 'NONE', #17733, #3317 ) ;
#26787 = CARTESIAN_POINT ( 'NONE',  ( 158.0000000000013358, 78.55899957960562574, -45.00000000000000000 ) ) ;
#26788 = CARTESIAN_POINT ( 'NONE',  ( 137.6591494508433300, 249.8824263794485319, -139.6178255645964725 ) ) ;
#26789 = VERTEX_POINT ( 'NONE', #20828 ) ;
#26790 = DIRECTION ( 'NONE',  ( 0.6681556583950252204, 0.7440215159218921404, 0.000000000000000000 ) ) ;
#26791 = EDGE_CURVE ( 'NONE', #23606, #20612, #27555, .T. ) ;
#26792 = ORIENTED_EDGE ( 'NONE', *, *, #26829, .F. ) ;
#26793 = AXIS2_PLACEMENT_3D ( 'NONE', #11049, #19803, #126 ) ;
#26794 = LINE ( 'NONE', #19752, #20316 ) ;
#26795 = VERTEX_POINT ( 'NONE', #12503 ) ;
#26796 = DIRECTION ( 'NONE',  ( 0.7440215159218921404, -0.6681556583950251094, 0.000000000000000000 ) ) ;
#26797 = ORIENTED_EDGE ( 'NONE', *, *, #17238, .T. ) ;
#26798 = VECTOR ( 'NONE', #8517, 1000.000000000000000 ) ;
#26799 = ORIENTED_EDGE ( 'NONE', *, *, #23039, .T. ) ;
#26800 = LINE ( 'NONE', #935, #14528 ) ;
#26801 = VERTEX_POINT ( 'NONE', #20682 ) ;
#26802 = EDGE_LOOP ( 'NONE', ( #2903, #7182, #4450, #10076 ) ) ;
#26803 = SHAPE_REPRESENTATION ( 'High-Force Electromagnet Base Block', ( #10637 ), #5568 ) ;
#26804 = ORIENTED_EDGE ( 'NONE', *, *, #22187, .T. ) ;
#26805 = EDGE_CURVE ( 'NONE', #15968, #14227, #24182, .T. ) ;
#26806 = CARTESIAN_POINT ( 'NONE',  ( 93.32984351717924199, 231.0185867901168137, 18.11991709984934573 ) ) ;
#26807 = EDGE_CURVE ( 'NONE', #19092, #13809, #21246, .T. ) ;
#26808 = DIRECTION ( 'NONE',  ( 0.000000000000000000, 0.000000000000000000, -1.000000000000000000 ) ) ;
#26809 = CARTESIAN_POINT ( 'NONE',  ( -229.2498027451138967, 132.0565166830976978, -15.00000000000000000 ) ) ;
#26810 = AXIS2_PLACEMENT_3D ( 'NONE', #23306, #21570, #1883 ) ;
#26811 = CARTESIAN_POINT ( 'NONE',  ( 52.57751368840760620, 248.9624084326366358, 45.00000000000000000 ) ) ;
#26812 = LINE ( 'NONE', #2958, #17223 ) ;
#26813 = DIRECTION ( 'NONE',  ( -8.673617379884073683E-17, -1.000000000000000000, 0.000000000000000000 ) ) ;
#26814 = DIRECTION ( 'NONE',  ( 0.05364526231779759985, 0.9985600561963485777, 0.000000000000000000 ) ) ;
#26815 = CARTESIAN_POINT ( 'NONE',  ( 158.0000000000011369, 96.11412463215494029, -45.00000000000000000 ) ) ;
#26816 = AXIS2_PLACEMENT_3D ( 'NONE', #26248, #13196, #18212 ) ;
#26817 = DIRECTION ( 'NONE',  ( -0.000000000000000000, -0.000000000000000000, -1.000000000000000000 ) ) ;
#26818 = CARTESIAN_POINT ( 'NONE',  ( 65.00000000000000000, -120.0000000000000995, -76.02499999999999147 ) ) ;
#26819 = CARTESIAN_POINT ( 'NONE',  ( 158.0000000000016769, 45.95662448201407102, 45.00000000000000000 ) ) ;
#26820 = ORIENTED_EDGE ( 'NONE', *, *, #26243, .T. ) ;
#26821 = SPHERICAL_SURFACE ( 'NONE', #17463, 35.18636678425505693 ) ;
#26822 = ADVANCED_FACE ( 'NONE', ( #27416 ), #10056, .F. ) ;
#26823 = DIRECTION ( 'NONE',  ( 0.000000000000000000, 0.000000000000000000, -1.000000000000000000 ) ) ;
#26824 = LINE ( 'NONE', #9159, #9395 ) ;
#26825 = CARTESIAN_POINT ( 'NONE',  ( 267.4999999999996021, 194.4107529906318348, -75.35061095560291733 ) ) ;
#26826 = EDGE_LOOP ( 'NONE', ( #7252, #293, #18665, #17896 ) ) ;
#26827 = CARTESIAN_POINT ( 'NONE',  ( 158.0000000000014211, 68.52749954957745615, -45.00000000000000000 ) ) ;
#26828 = ORIENTED_EDGE ( 'NONE', *, *, #17431, .T. ) ;
#26829 = EDGE_CURVE ( 'NONE', #15645, #970, #15023, .T. ) ;
#26830 = CARTESIAN_POINT ( 'NONE',  ( -40.40953891503691153, 0.000000000000000000, 99.00000000000000000 ) ) ;
#26831 = ORIENTED_EDGE ( 'NONE', *, *, #23822, .F. ) ;
#26832 = ORIENTED_EDGE ( 'NONE', *, *, #25355, .T. ) ;
#26833 = ORIENTED_EDGE ( 'NONE', *, *, #5425, .F. ) ;
#26834 = EDGE_CURVE ( 'NONE', #13479, #14223, #5873, .T. ) ;
#26835 = ORIENTED_EDGE ( 'NONE', *, *, #21691, .T. ) ;
#26836 = CARTESIAN_POINT ( 'NONE',  ( -190.0000000000000284, 59.99999999999995026, 110.0000000000000284 ) ) ;
#26837 = LINE ( 'NONE', #7305, #12304 ) ;
#26838 = DIRECTION ( 'NONE',  ( 8.659560562354934091E-17, 0.7071067811865474617, -0.7071067811865476838 ) ) ;
#26839 = ADVANCED_FACE ( 'NONE', ( #16526 ), #25134, .F. ) ;
#26840 = EDGE_CURVE ( 'NONE', #9674, #4623, #5734, .T. ) ;
#26841 = DIRECTION ( 'NONE',  ( 1.000000000000000000, -0.000000000000000000, -0.000000000000000000 ) ) ;
#26842 = LINE ( 'NONE', #22821, #2469 ) ;
#26843 = CARTESIAN_POINT ( 'NONE',  ( -230.0306293838742988, 64.31401865985674249, 16.82661551914410225 ) ) ;
#26844 = CARTESIAN_POINT ( 'NONE',  ( 157.4999999999998579, 163.5728123310915407, 45.00000000000000000 ) ) ;
#26845 = DIRECTION ( 'NONE',  ( -0.000000000000000000, -0.000000000000000000, -1.000000000000000000 ) ) ;
#26846 = DIRECTION ( 'NONE',  ( -1.000000000000000000, -0.000000000000000000, -0.000000000000000000 ) ) ;
#26847 = VECTOR ( 'NONE', #19491, 1000.000000000000000 ) ;
#26848 = CARTESIAN_POINT ( 'NONE',  ( 294.9233831825460470, 127.6681916698403114, -153.0000000000000000 ) ) ;
#26849 = CARTESIAN_POINT ( 'NONE',  ( 158.0000000000013074, 81.06687458711267880, -45.00000000000000000 ) ) ;
#26850 = PLANE ( 'NONE',  #18716 ) ;
#26851 = CARTESIAN_POINT ( 'NONE',  ( 108.2273028572102760, 129.5338070841179672, 88.59375000028596503 ) ) ;
#26852 = VECTOR ( 'NONE', #20204, 1000.000000000000000 ) ;
#26853 = CARTESIAN_POINT ( 'NONE',  ( -13.62884545128598823, 130.9145211729554603, 16.37206327941867201 ) ) ;
#26854 = CARTESIAN_POINT ( 'NONE',  ( 167.4999999999996589, 258.6181251126050711, 6.000000000000019540 ) ) ;
#26855 = DIRECTION ( 'NONE',  ( -0.2588190451024993122, 0.9659258262890740854, 0.000000000000000000 ) ) ;
#26856 = DIRECTION ( 'NONE',  ( 0.8916010070290389944, -0.4528218681389001854, 0.000000000000000000 ) ) ;
#26857 = AXIS2_PLACEMENT_3D ( 'NONE', #7505, #1163, #14254 ) ;
#26859 = ORIENTED_EDGE ( 'NONE', *, *, #28135, .F. ) ;
#26858 = VERTEX_POINT ( 'NONE', #7760 ) ;
#26860 = CARTESIAN_POINT ( 'NONE',  ( -200.0000000000000284, -91.18033988749901653, 0.000000000000000000 ) ) ;
#26861 = CARTESIAN_POINT ( 'NONE',  ( 33.10302365956999182, 203.2034914284457159, 15.00000000000000000 ) ) ;
#26862 = ORIENTED_EDGE ( 'NONE', *, *, #5827, .F. ) ;
#26863 = VERTEX_POINT ( 'NONE', #14513 ) ;
#26864 = ORIENTED_EDGE ( 'NONE', *, *, #20118, .F. ) ;
#26865 = EDGE_CURVE ( 'NONE', #19837, #18244, #7227, .T. ) ;
#26866 = LINE ( 'NONE', #20399, #26704 ) ;
#26867 = LINE ( 'NONE', #588, #18187 ) ;
#26868 = VERTEX_POINT ( 'NONE', #27701 ) ;
#26869 = AXIS2_PLACEMENT_3D ( 'NONE', #24054, #21755, #24322 ) ;
#26870 = ORIENTED_EDGE ( 'NONE', *, *, #15072, .F. ) ;
#26871 = LINE ( 'NONE', #7199, #7401 ) ;
#26872 = VECTOR ( 'NONE', #25362, 1000.000000000000114 ) ;
#26873 = VECTOR ( 'NONE', #24644, 1000.000000000000000 ) ;
#26874 = DIRECTION ( 'NONE',  ( -1.321694076934710155E-16, 1.000000000000000000, 0.000000000000000000 ) ) ;
#26875 = ADVANCED_FACE ( 'NONE', ( #18955 ), #10197, .T. ) ;
#26876 = DIRECTION ( 'NONE',  ( 1.000000000000000000, -0.000000000000000000, -0.000000000000000000 ) ) ;
#26877 = ORIENTED_EDGE ( 'NONE', *, *, #11713, .T. ) ;
#26878 = SURFACE_SIDE_STYLE ('',( #5033 ) ) ;
#26879 = VECTOR ( 'NONE', #14691, 1000.000000000000000 ) ;
#26880 = CARTESIAN_POINT ( 'NONE',  ( 157.4999999999998295, 231.2854375337815327, 45.00000000000000000 ) ) ;
#26881 = EDGE_CURVE ( 'NONE', #17566, #6716, #16390, .T. ) ;
#26882 = DIRECTION ( 'NONE',  ( -0.8916010070299882351, -0.4528218681370311249, 0.000000000000000000 ) ) ;
#26883 = FACE_OUTER_BOUND ( 'NONE', #17354, .T. ) ;
#26884 = CARTESIAN_POINT ( 'NONE',  ( -210.9349024751243178, 73.41979635535319915, -32.58420779144454826 ) ) ;
#26885 = ORIENTED_EDGE ( 'NONE', *, *, #12010, .F. ) ;
#26886 = LINE ( 'NONE', #13539, #858 ) ;
#26887 = VECTOR ( 'NONE', #26845, 1000.000000000000000 ) ;
#26888 = CARTESIAN_POINT ( 'NONE',  ( -229.2498027451138967, 132.0565166830976978, -15.00000000000000178 ) ) ;
#26889 = DIRECTION ( 'NONE',  ( 0.2588190451025121908, -0.9659258262890705327, 0.000000000000000000 ) ) ;
#26890 = CARTESIAN_POINT ( 'NONE',  ( 158.0000000000008242, 128.2086247222394206, -45.00000000000000000 ) ) ;
#26891 = ORIENTED_EDGE ( 'NONE', *, *, #24433, .T. ) ;
#26892 = VECTOR ( 'NONE', #18981, 1000.000000000000000 ) ;
#26893 = CARTESIAN_POINT ( 'NONE',  ( 154.8288972274760908, 222.6105238444010297, 45.00000000000000000 ) ) ;
#26894 = LINE ( 'NONE', #20284, #21205 ) ;
#26895 = CARTESIAN_POINT ( 'NONE',  ( -143.2374437020967264, 68.51688903468615877, 83.00000000000001421 ) ) ;
#26896 = VERTEX_POINT ( 'NONE', #16803 ) ;
#26897 = CIRCLE ( 'NONE', #286, 7.999999999999979572 ) ;
#26898 = ORIENTED_EDGE ( 'NONE', *, *, #27579, .T. ) ;
#26899 = EDGE_CURVE ( 'NONE', #24769, #24234, #3088, .T. ) ;
#26900 = LINE ( 'NONE', #27307, #24870 ) ;
#26901 = CARTESIAN_POINT ( 'NONE',  ( 157.9999999999996874, 269.1575001501400379, -45.00000000000000000 ) ) ;
#26902 = ORIENTED_EDGE ( 'NONE', *, *, #20263, .T. ) ;
#26903 = ORIENTED_EDGE ( 'NONE', *, *, #3439, .T. ) ;
#26904 = FACE_OUTER_BOUND ( 'NONE', #26905, .T. ) ;
#26905 = EDGE_LOOP ( 'NONE', ( #5636, #13746, #11869, #7824, #8525, #10494, #19642, #6992, #13455, #8458, #551, #24304, #9837, #17161, #18189, #14060, #12005, #22646, #4830, #19438, #14720, #22189, #5483, #5439, #25303, #20440, #7369, #24957, #25650, #8244, #15313, #3947, #14065, #22167, #10501, #6786, #26903, #27584, #21944, #9741, #24278, #20984, #10542, #20435, #25268, #2490, #11620, #7613, #23096, #25715, #2870, #1719, #24389, #19025, #10425, #25761, #694, #25550, #8954, #25127, #14925, #3990, #9370, #6495, #1869, #21422, #6740, #24509, #5947, #7721, #16861, #15643 ) ) ;
#26906 = DIRECTION ( 'NONE',  ( 0.000000000000000000, 0.000000000000000000, 1.000000000000000000 ) ) ;
#26907 = ORIENTED_EDGE ( 'NONE', *, *, #6659, .F. ) ;
#26908 = AXIS2_PLACEMENT_3D ( 'NONE', #22917, #22780, #9567 ) ;
#26909 = CARTESIAN_POINT ( 'NONE',  ( 157.4999999999998579, 221.2539375037535194, -45.00000000000000000 ) ) ;
#26910 = ADVANCED_FACE ( 'NONE', ( #25001 ), #14097, .F. ) ;
#26911 = EDGE_CURVE ( 'NONE', #5065, #1176, #12926, .T. ) ;
#26912 = CARTESIAN_POINT ( 'NONE',  ( 157.9999999999996874, 266.6496251426330559, 45.00000000000000000 ) ) ;
#26913 = DIRECTION ( 'NONE',  ( 0.8916010070298860946, -0.4528218681372321863, 0.000000000000000000 ) ) ;
#26914 = CARTESIAN_POINT ( 'NONE',  ( 1.655276743323666810, 135.1741146306952430, -15.36901953696933987 ) ) ;
#26915 = CIRCLE ( 'NONE', #9937, 1.999999999999994893 ) ;
#26916 = DIRECTION ( 'NONE',  ( 0.8018642810807398158, 0.5975062131282554700, -0.000000000000000000 ) ) ;
#26917 = LINE ( 'NONE', #24623, #4142 ) ;
#26918 = DIRECTION ( 'NONE',  ( 1.000000000000000000, 0.000000000000000000, -0.000000000000000000 ) ) ;
#26919 = ORIENTED_EDGE ( 'NONE', *, *, #19261, .F. ) ;
#26920 = DIRECTION ( 'NONE',  ( 0.000000000000000000, 0.000000000000000000, -1.000000000000000000 ) ) ;
#26921 = FACE_OUTER_BOUND ( 'NONE', #7829, .T. ) ;
#26922 = LINE ( 'NONE', #7101, #26089 ) ;
#26923 = DIRECTION ( 'NONE',  ( 1.000000000000000000, 0.000000000000000000, 0.000000000000000000 ) ) ;
#26924 = VERTEX_POINT ( 'NONE', #4424 ) ;
#26925 = ADVANCED_FACE ( 'NONE', ( #3860 ), #8747, .F. ) ;
#26926 = LINE ( 'NONE', #20462, #10063 ) ;
#26927 = ORIENTED_EDGE ( 'NONE', *, *, #28271, .F. ) ;
#26928 = EDGE_CURVE ( 'NONE', #13840, #11731, #19377, .T. ) ;
#26929 = LINE ( 'NONE', #16165, #4273 ) ;
#26930 = CARTESIAN_POINT ( 'NONE',  ( -224.2511286692390229, 62.13136325095025825, -9.143584677369513969 ) ) ;
#26931 = CARTESIAN_POINT ( 'NONE',  ( 136.9357406746122479, 249.9396928751734492, -139.3072807822095740 ) ) ;
#26932 = ORIENTED_EDGE ( 'NONE', *, *, #7639, .T. ) ;
#26933 = FACE_OUTER_BOUND ( 'NONE', #28149, .T. ) ;
#26934 = ORIENTED_EDGE ( 'NONE', *, *, #2297, .F. ) ;
#26935 = AXIS2_PLACEMENT_3D ( 'NONE', #763, #9529, #27039 ) ;
#26936 = LINE ( 'NONE', #20610, #15287 ) ;
#26937 = ORIENTED_EDGE ( 'NONE', *, *, #17860, .F. ) ;
#26938 = PLANE ( 'NONE',  #17244 ) ;
#26939 = EDGE_LOOP ( 'NONE', ( #12572, #13416, #10265, #14027 ) ) ;
#26940 = EDGE_CURVE ( 'NONE', #16172, #15403, #27981, .T. ) ;
#26941 = EDGE_LOOP ( 'NONE', ( #8535, #6657, #16787, #17992 ) ) ;
#26942 = CARTESIAN_POINT ( 'NONE',  ( 115.1711027725237528, 222.6105238444006886, 45.00000000000000000 ) ) ;
#26943 = VERTEX_POINT ( 'NONE', #19659 ) ;
#26944 = ORIENTED_EDGE ( 'NONE', *, *, #18787, .T. ) ;
#26945 = ORIENTED_EDGE ( 'NONE', *, *, #1695, .T. ) ;
#26946 = CARTESIAN_POINT ( 'NONE',  ( -175.0000000000000000, -170.0000000000001705, 64.00000000000004263 ) ) ;
#26947 = FACE_OUTER_BOUND ( 'NONE', #9812, .T. ) ;
#26948 = DIRECTION ( 'NONE',  ( -0.000000000000000000, 1.000000000000000000, -1.387778780781445429E-16 ) ) ;
#26949 = CIRCLE ( 'NONE', #21446, 5.000000000000004441 ) ;
#26950 = CARTESIAN_POINT ( 'NONE',  ( 109.9999999999999147, 137.0808454112663810, -89.99999999930710715 ) ) ;
#26951 = FACE_OUTER_BOUND ( 'NONE', #18491, .T. ) ;
#26952 = CARTESIAN_POINT ( 'NONE',  ( 8.117852850209656523, 141.5785587194356481, 12.99999999999999822 ) ) ;
#26953 = DIRECTION ( 'NONE',  ( -0.000000000000000000, -0.000000000000000000, 1.000000000000000000 ) ) ;
#26954 = CARTESIAN_POINT ( 'NONE',  ( 87.50000000000029843, 230.0000000000000284, -15.95262490344447492 ) ) ;
#26955 = CARTESIAN_POINT ( 'NONE',  ( 282.4999999999996589, 19.41075299063184900, 87.99671038392668265 ) ) ;
#26956 = DIRECTION ( 'NONE',  ( 1.000000000000000000, 0.000000000000000000, 0.000000000000000000 ) ) ;
#26957 = DIRECTION ( 'NONE',  ( -0.7123733896039576852, -0.6147814225729698601, -0.3384788859638417913 ) ) ;
#26958 = EDGE_LOOP ( 'NONE', ( #9944, #27735, #20171, #27546, #24818, #26082, #18768, #23260 ) ) ;
#26959 = CARTESIAN_POINT ( 'NONE',  ( 111.9999999999999574, 220.9999999999996874, 45.00000000000000000 ) ) ;
#26960 = CARTESIAN_POINT ( 'NONE',  ( 187.4999999999996305, 83.06687458711267880, 36.86484227207694175 ) ) ;
#26961 = CYLINDRICAL_SURFACE ( 'NONE', #2962, 5.999999999999991118 ) ;
#26962 = CARTESIAN_POINT ( 'NONE',  ( 158.0000000000005116, 158.8109998198309825, 45.00000000000000000 ) ) ;
#26963 = ORIENTED_EDGE ( 'NONE', *, *, #5150, .F. ) ;
#26964 = EDGE_CURVE ( 'NONE', #12431, #19520, #6017, .T. ) ;
#26965 = AXIS2_PLACEMENT_3D ( 'NONE', #11949, #13827, #7352 ) ;
#26966 = DIRECTION ( 'NONE',  ( 0.8916010070298658885, -0.4528218681372722099, 0.000000000000000000 ) ) ;
#26967 = ORIENTED_EDGE ( 'NONE', *, *, #25656, .T. ) ;
#26968 =( NAMED_UNIT ( * ) PLANE_ANGLE_UNIT ( ) SI_UNIT ( $, .RADIAN. ) );
#26969 = EDGE_CURVE ( 'NONE', #17314, #883, #14795, .T. ) ;
#26970 = ORIENTED_EDGE ( 'NONE', *, *, #16374, .F. ) ;
#26971 = ORIENTED_EDGE ( 'NONE', *, *, #24973, .F. ) ;
#26972 = ORIENTED_EDGE ( 'NONE', *, *, #23624, .F. ) ;
#26973 = EDGE_LOOP ( 'NONE', ( #7709, #21973, #8318, #14224 ) ) ;
#26974 = CARTESIAN_POINT ( 'NONE',  ( -160.8326600028555902, 120.2355194873575073, 21.37420696376536711 ) ) ;
#26975 = LINE ( 'NONE', #18082, #3314 ) ;
#26976 = CARTESIAN_POINT ( 'NONE',  ( -62.43823629548968768, 134.9066984251663825, -13.78087915458745627 ) ) ;
#26977 = CARTESIAN_POINT ( 'NONE',  ( 33.10302365956999182, 203.2034914284457159, -13.00000000000000000 ) ) ;
#26978 = CARTESIAN_POINT ( 'NONE',  ( -195.7913036700337841, 62.61587363931871408, 36.00381397819591456 ) ) ;
#26980 = LINE ( 'NONE', #7020, #4819 ) ;
#26979 = VECTOR ( 'NONE', #4149, 1000.000000000000000 ) ;
#26981 = CARTESIAN_POINT ( 'NONE',  ( -62.43610812620287476, 134.9063932224630094, -13.78094890389263938 ) ) ;
#26982 = EDGE_CURVE ( 'NONE', #13811, #23117, #6298, .T. ) ;
#26983 = LINE ( 'NONE', #9756, #17249 ) ;
#26984 = VECTOR ( 'NONE', #22327, 1000.000000000000000 ) ;
#26985 = DIRECTION ( 'NONE',  ( 0.000000000000000000, -1.000000000000000000, 0.000000000000000000 ) ) ;
#26986 = FACE_OUTER_BOUND ( 'NONE', #17440, .T. ) ;
#26987 = CARTESIAN_POINT ( 'NONE',  ( 217.4999999999996305, 83.06687458711267880, 36.86484227207694175 ) ) ;
#26988 = DIRECTION ( 'NONE',  ( 1.000000000000000000, 1.321694076934710155E-16, 0.000000000000000000 ) ) ;
#26989 = CARTESIAN_POINT ( 'NONE',  ( 0.8462782258048142658, 136.6959233578304236, 15.12258877882598007 ) ) ;
#26990 = CARTESIAN_POINT ( 'NONE',  ( -260.0000000000001137, -167.0819201924624906, -89.99999999999985789 ) ) ;
#26991 = CARTESIAN_POINT ( 'NONE',  ( 187.4999999999996305, 494.4107529906318632, -100.0000000000000142 ) ) ;
#26992 = EDGE_CURVE ( 'NONE', #4186, #13809, #5391, .T. ) ;
#26993 = CARTESIAN_POINT ( 'NONE',  ( 65.00000000000000000, -120.0000000000000995, -69.99999999999998579 ) ) ;
#26995 = ORIENTED_EDGE ( 'NONE', *, *, #16660, .F. ) ;
#26994 = VERTEX_POINT ( 'NONE', #13209 ) ;
#26996 = CARTESIAN_POINT ( 'NONE',  ( -217.9749057636497582, 86.24598930254806817, -19.84474727259476978 ) ) ;
#26997 = EDGE_CURVE ( 'NONE', #11481, #11333, #17776, .T. ) ;
#26998 = EDGE_CURVE ( 'NONE', #18102, #8949, #19153, .T. ) ;
#26999 = CARTESIAN_POINT ( 'NONE',  ( 157.4999999999994600, 216.2381874887387880, 45.00000000000000000 ) ) ;
#27000 = EDGE_CURVE ( 'NONE', #2647, #14369, #23835, .T. ) ;
#27001 = VERTEX_POINT ( 'NONE', #6165 ) ;
#27002 = VERTEX_POINT ( 'NONE', #19523 ) ;
#27003 = VECTOR ( 'NONE', #16611, 1000.000000000000000 ) ;
#27004 = PLANE ( 'NONE',  #18476 ) ;
#27005 = CARTESIAN_POINT ( 'NONE',  ( -135.0977962388534763, 129.7097216771591661, 16.78759912078217553 ) ) ;
#27006 = VECTOR ( 'NONE', #11270, 1000.000000000000000 ) ;
#27007 = ORIENTED_EDGE ( 'NONE', *, *, #14742, .F. ) ;
#27008 = VERTEX_POINT ( 'NONE', #25980 ) ;
#27009 = DIRECTION ( 'NONE',  ( 0.8916010070293783896, -0.4528218681382319422, 0.000000000000000000 ) ) ;
#27010 = CARTESIAN_POINT ( 'NONE',  ( 187.4999999999996305, 288.9665627064425166, 45.00000000000000000 ) ) ;
#27011 = DIRECTION ( 'NONE',  ( -0.000000000000000000, -0.000000000000000000, -1.000000000000000000 ) ) ;
#27012 = LINE ( 'NONE', #9214, #11926 ) ;
#27013 = DIRECTION ( 'NONE',  ( -0.8916010070293547418, -0.4528218681382785715, 0.000000000000000000 ) ) ;
#27014 = VECTOR ( 'NONE', #7105, 1000.000000000000227 ) ;
#27015 = DIRECTION ( 'NONE',  ( 0.8916010070298766577, 0.4528218681372509491, 0.000000000000000000 ) ) ;
#27016 = LINE ( 'NONE', #13972, #25174 ) ;
#27017 = CARTESIAN_POINT ( 'NONE',  ( -214.0051257764050945, 55.38571953469315901, -43.60894023861363422 ) ) ;
#27018 = CIRCLE ( 'NONE', #14645, 7.685040811306672381 ) ;
#27019 = EDGE_CURVE ( 'NONE', #3365, #20790, #19799, .T. ) ;
#27020 = CARTESIAN_POINT ( 'NONE',  ( 167.4999999999996589, 526.4263741777961059, -84.99999999999995737 ) ) ;
#27021 = ADVANCED_BREP_SHAPE_REPRESENTATION ( '', ( #28013, #10637 ), #15244 ) ;
#27022 = LINE ( 'NONE', #17985, #8324 ) ;
#27023 = DIRECTION ( 'NONE',  ( 1.000000000000000000, 0.000000000000000000, 0.000000000000000000 ) ) ;
#27024 = CARTESIAN_POINT ( 'NONE',  ( 124.9999999999998579, 220.0000000000000284, 90.00000000000002842 ) ) ;
#27025 = ORIENTED_EDGE ( 'NONE', *, *, #11675, .T. ) ;
#27026 = DIRECTION ( 'NONE',  ( -0.8660254037844362651, 0.5000000000000039968, -0.000000000000000000 ) ) ;
#27027 = CONICAL_SURFACE ( 'NONE', #5920, 6.025000000000002132, 0.7853981633974482790 ) ;
#27028 = EDGE_CURVE ( 'NONE', #7114, #15531, #26949, .T. ) ;
#27029 = DIRECTION ( 'NONE',  ( 0.9960550913260673989, 1.086714821493789192E-17, 0.08873699929240025375 ) ) ;
#27030 = CARTESIAN_POINT ( 'NONE',  ( 157.9999999999998295, 226.0157500150140208, 45.00000000000000000 ) ) ;
#27031 = ORIENTED_EDGE ( 'NONE', *, *, #12376, .T. ) ;
#27032 = VERTEX_POINT ( 'NONE', #6445 ) ;
#27033 = CARTESIAN_POINT ( 'NONE',  ( 157.9999999999996874, 266.1417501351260171, -45.00000000000000000 ) ) ;
#27034 = VECTOR ( 'NONE', #17876, 1000.000000000000000 ) ;
#27035 = LINE ( 'NONE', #4621, #8062 ) ;
#27036 = ORIENTED_EDGE ( 'NONE', *, *, #11141, .T. ) ;
#27037 = VECTOR ( 'NONE', #27183, 1000.000000000000000 ) ;
#27038 = ORIENTED_EDGE ( 'NONE', *, *, #1996, .T. ) ;
#27039 = DIRECTION ( 'NONE',  ( 0.000000000000000000, 0.000000000000000000, -1.000000000000000000 ) ) ;
#27040 = CIRCLE ( 'NONE', #10518, 5.000000000000004441 ) ;
#27041 = PLANE ( 'NONE',  #5156 ) ;
#27042 = DIRECTION ( 'NONE',  ( -0.000000000000000000, -0.000000000000000000, -1.000000000000000000 ) ) ;
#27043 = ORIENTED_EDGE ( 'NONE', *, *, #22299, .T. ) ;
#27044 = FACE_OUTER_BOUND ( 'NONE', #14013, .T. ) ;
#27045 = ORIENTED_EDGE ( 'NONE', *, *, #14019, .F. ) ;
#27046 = LINE ( 'NONE', #1185, #5643 ) ;
#27047 = VECTOR ( 'NONE', #10199, 1000.000000000000000 ) ;
#27048 = CARTESIAN_POINT ( 'NONE',  ( 157.4999999999998579, 80.81293708335913095, 45.00000000000000000 ) ) ;
#27049 = LINE ( 'NONE', #20722, #3870 ) ;
#27050 = CARTESIAN_POINT ( 'NONE',  ( -22.99863117501815069, 128.1622734824785823, -17.43423781283663132 ) ) ;
#27051 = CARTESIAN_POINT ( 'NONE',  ( 0.000000000000000000, 1.249999999999999556, -6.997769477110050929 ) ) ;
#27052 = CARTESIAN_POINT ( 'NONE',  ( 157.9999999999996305, 286.7126252026890256, 45.00000000000000000 ) ) ;
#27053 = CARTESIAN_POINT ( 'NONE',  ( 157.4999999999998579, 83.32081209086616980, 45.00000000000000000 ) ) ;
#27054 = ADVANCED_FACE ( 'NONE', ( #15223 ), #21954, .T. ) ;
#27055 = VERTEX_POINT ( 'NONE', #2263 ) ;
#27056 = AXIS2_PLACEMENT_3D ( 'NONE', #6418, #9001, #28369 ) ;
#27057 = CARTESIAN_POINT ( 'NONE',  ( 157.9999999999996589, 271.6653751576470768, -45.00000000000000000 ) ) ;
#27058 = CARTESIAN_POINT ( 'NONE',  ( -227.3657730843237346, 133.9833936510272565, 14.99191580167116733 ) ) ;
#27059 = DIRECTION ( 'NONE',  ( 0.000000000000000000, -1.000000000000000000, 0.000000000000000000 ) ) ;
#27060 = CARTESIAN_POINT ( 'NONE',  ( 157.4999999999998579, 143.5098122710352015, 45.00000000000000000 ) ) ;
#27061 = ORIENTED_EDGE ( 'NONE', *, *, #16016, .T. ) ;
#27062 = DIRECTION ( 'NONE',  ( -1.000000000000000000, 5.551115123125784674E-16, 0.000000000000000000 ) ) ;
#27063 = VECTOR ( 'NONE', #25966, 1000.000000000000114 ) ;
#27064 = ORIENTED_EDGE ( 'NONE', *, *, #1571, .T. ) ;
#27065 = CARTESIAN_POINT ( 'NONE',  ( 74.37710191228967460, 227.8920494084358950, -45.00000000000000000 ) ) ;
#27066 = CARTESIAN_POINT ( 'NONE',  ( 157.4999999999998579, 88.33656210588026170, -45.00000000000000000 ) ) ;
#27067 = FACE_OUTER_BOUND ( 'NONE', #13091, .T. ) ;
#27068 = ORIENTED_EDGE ( 'NONE', *, *, #2890, .T. ) ;
#27069 = PLANE ( 'NONE',  #17960 ) ;
#27070 = FACE_OUTER_BOUND ( 'NONE', #5373, .T. ) ;
#27071 = VERTEX_POINT ( 'NONE', #23693 ) ;
#27072 = EDGE_CURVE ( 'NONE', #16719, #999, #1274, .T. ) ;
#27073 = CARTESIAN_POINT ( 'NONE',  ( 157.9999999999997442, 251.0945000900840398, 45.00000000000000000 ) ) ;
#27074 = EDGE_CURVE ( 'NONE', #27404, #9161, #4001, .T. ) ;
#27075 = CARTESIAN_POINT ( 'NONE',  ( 96.24937469161466197, 240.9969810907205954, 9.998609732053244770 ) ) ;
#27076 = VERTEX_POINT ( 'NONE', #28398 ) ;
#27077 = EDGE_LOOP ( 'NONE', ( #21985, #2952, #21345, #27413 ) ) ;
#27078 = DIRECTION ( 'NONE',  ( 1.000000000000000000, 0.000000000000000000, -0.000000000000000000 ) ) ;
#27079 = ORIENTED_EDGE ( 'NONE', *, *, #13652, .T. ) ;
#27080 = AXIS2_PLACEMENT_3D ( 'NONE', #12900, #23243, #25530 ) ;
#27081 = EDGE_LOOP ( 'NONE', ( #8885, #6971, #17419, #3109, #15607 ) ) ;
#27082 = EDGE_LOOP ( 'NONE', ( #26183, #3357, #13206, #25345, #25075, #11567, #6481, #19796 ) ) ;
#27083 = EDGE_CURVE ( 'NONE', #19656, #9422, #20081, .T. ) ;
#27084 = DIRECTION ( 'NONE',  ( 1.000000000000000000, 0.000000000000000000, 0.000000000000000000 ) ) ;
#27085 = AXIS2_PLACEMENT_3D ( 'NONE', #16307, #10117, #25475 ) ;
#27086 = EDGE_CURVE ( 'NONE', #152, #11767, #19943, .T. ) ;
#27087 = DIRECTION ( 'NONE',  ( 0.4528218681382713551, -0.8916010070293584056, 0.000000000000000000 ) ) ;
#27088 = CARTESIAN_POINT ( 'NONE',  ( 157.4999999999998579, 115.9231871884577174, -45.00000000000000000 ) ) ;
#27089 = CARTESIAN_POINT ( 'NONE',  ( 157.4999999999998579, 68.27356204582390831, 45.00000000000000000 ) ) ;
#27090 = CARTESIAN_POINT ( 'NONE',  ( 179.9999999999999147, 494.4107529906318632, 100.0000000000000142 ) ) ;
#27091 = DIRECTION ( 'NONE',  ( -0.000000000000000000, 0.000000000000000000, -1.000000000000000000 ) ) ;
#27092 = CARTESIAN_POINT ( 'NONE',  ( 141.9187638636469160, 241.9574749595457774, 45.00000000000000000 ) ) ;
#27093 = LINE ( 'NONE', #26815, #20901 ) ;
#27094 = CARTESIAN_POINT ( 'NONE',  ( -273.2648702738334237, -170.0373740213163103, 108.3066405192712267 ) ) ;
#27095 = LINE ( 'NONE', #26513, #21955 ) ;
#27096 = FACE_OUTER_BOUND ( 'NONE', #22668, .T. ) ;
#27097 = VERTEX_POINT ( 'NONE', #2696 ) ;
#27098 = VECTOR ( 'NONE', #21464, 1000.000000000000000 ) ;
#27099 = DIRECTION ( 'NONE',  ( 0.4528218681378110011, 0.8916010070295922185, -0.000000000000000000 ) ) ;
#27100 = PLANE ( 'NONE',  #25433 ) ;
#27101 = CARTESIAN_POINT ( 'NONE',  ( 158.0000000000003126, 176.3661248723802828, 45.00000000000000000 ) ) ;
#27102 = ORIENTED_EDGE ( 'NONE', *, *, #2904, .F. ) ;
#27103 = EDGE_CURVE ( 'NONE', #14397, #3747, #4458, .T. ) ;
#27104 = AXIS2_PLACEMENT_3D ( 'NONE', #4045, #12555, #21296 ) ;
#27105 = EDGE_CURVE ( 'NONE', #18947, #23572, #9468, .T. ) ;
#27106 = DIRECTION ( 'NONE',  ( -0.2066290158914688424, -0.9784193629480781862, 0.000000000000000000 ) ) ;
#27107 = EDGE_LOOP ( 'NONE', ( #14064, #23251, #2004, #9207 ) ) ;
#27108 = DIRECTION ( 'NONE',  ( -0.000000000000000000, -0.000000000000000000, 1.000000000000000000 ) ) ;
#27109 = ORIENTED_EDGE ( 'NONE', *, *, #12066, .F. ) ;
#27110 = ORIENTED_EDGE ( 'NONE', *, *, #2928, .F. ) ;
#27111 = ORIENTED_EDGE ( 'NONE', *, *, #26732, .F. ) ;
#27112 = ORIENTED_EDGE ( 'NONE', *, *, #8640, .T. ) ;
#27113 = DIRECTION ( 'NONE',  ( -0.000000000000000000, -0.000000000000000000, -1.000000000000000000 ) ) ;
#27114 = EDGE_CURVE ( 'NONE', #3882, #8550, #17646, .T. ) ;
#27115 = DIRECTION ( 'NONE',  ( 0.000000000000000000, 0.000000000000000000, 1.000000000000000000 ) ) ;
#27116 = FACE_OUTER_BOUND ( 'NONE', #18034, .T. ) ;
#27117 = VECTOR ( 'NONE', #6061, 999.9999999999998863 ) ;
#27118 = CARTESIAN_POINT ( 'NONE',  ( 157.4999999999996589, 281.4429376839215138, 45.00000000000000000 ) ) ;
#27119 = EDGE_CURVE ( 'NONE', #6791, #23180, #9032, .T. ) ;
#27120 = LINE ( 'NONE', #2702, #25414 ) ;
#27121 = EDGE_CURVE ( 'NONE', #502, #19228, #4705, .T. ) ;
#27122 = CIRCLE ( 'NONE', #15207, 3.532530335305414493 ) ;
#27123 = CARTESIAN_POINT ( 'NONE',  ( -207.6173544636101553, 75.51556044650348554, 42.73482814336003344 ) ) ;
#27124 = CARTESIAN_POINT ( 'NONE',  ( 157.9999999999998010, 238.5551250525490161, 45.00000000000000000 ) ) ;
#27125 = CARTESIAN_POINT ( 'NONE',  ( -96.56864860929032091, 136.1733035486019787, -13.53429741579593681 ) ) ;
#27126 = CARTESIAN_POINT ( 'NONE',  ( 79.99999999999997158, 106.9649888129831794, -83.29453619103985318 ) ) ;
#27127 = CARTESIAN_POINT ( 'NONE',  ( 167.4999999999996589, 494.4107529906318632, -84.99999999999995737 ) ) ;
#27128 = EDGE_CURVE ( 'NONE', #12401, #11179, #24200, .T. ) ;
#27129 = LINE ( 'NONE', #2994, #10594 ) ;
#27130 = CARTESIAN_POINT ( 'NONE',  ( 157.4999999999998579, 130.9704372334999789, 45.00000000000000000 ) ) ;
#27131 = FACE_BOUND ( 'NONE', #21813, .T. ) ;
#27132 = CARTESIAN_POINT ( 'NONE',  ( -290.0000000000001137, -165.0000000000000853, 60.00000000000002842 ) ) ;
#27133 = CARTESIAN_POINT ( 'NONE',  ( -201.6741895288615183, 93.98653502690473260, 30.48002917746099172 ) ) ;
#27134 = CARTESIAN_POINT ( 'NONE',  ( -221.3650667873343139, -91.18033988749901653, 0.000000000000000000 ) ) ;
#27136 = ORIENTED_EDGE ( 'NONE', *, *, #27140, .T. ) ;
#27135 = ORIENTED_EDGE ( 'NONE', *, *, #11378, .T. ) ;
#27137 = AXIS2_PLACEMENT_3D ( 'NONE', #22077, #13760, #6844 ) ;
#27138 = CARTESIAN_POINT ( 'NONE',  ( -260.0000000000001137, -157.0000000000000284, -104.9999999999998721 ) ) ;
#27139 = ORIENTED_EDGE ( 'NONE', *, *, #16504, .T. ) ;
#27140 = EDGE_CURVE ( 'NONE', #3426, #18280, #26476, .T. ) ;
#27141 = VECTOR ( 'NONE', #21910, 1000.000000000000114 ) ;
#27142 = ORIENTED_EDGE ( 'NONE', *, *, #14327, .F. ) ;
#27143 = AXIS2_PLACEMENT_3D ( 'NONE', #23536, #28110, #15063 ) ;
#27144 = CARTESIAN_POINT ( 'NONE',  ( 134.9999999999998579, 220.0000000000000284, -90.00000000000002842 ) ) ;
#27145 = CARTESIAN_POINT ( 'NONE',  ( -82.76390570603551566, 134.7701287218720552, 15.45937173543416066 ) ) ;
#27146 = EDGE_LOOP ( 'NONE', ( #9092, #13782, #9466, #11799 ) ) ;
#27147 = VERTEX_POINT ( 'NONE', #4563 ) ;
#27148 = PLANE ( 'NONE',  #10115 ) ;
#27149 = CARTESIAN_POINT ( 'NONE',  ( -310.0000000000001137, -220.0000000000000853, 60.00000000000002842 ) ) ;
#27150 = DIRECTION ( 'NONE',  ( 0.000000000000000000, 0.000000000000000000, 1.000000000000000000 ) ) ;
#27151 = CARTESIAN_POINT ( 'NONE',  ( 94.28023193196015939, 231.3879991501505060, -18.61206014455101254 ) ) ;
#27152 = ADVANCED_FACE ( 'NONE', ( #22385 ), #9173, .F. ) ;
#27153 = ADVANCED_FACE ( 'NONE', ( #26683 ), #412, .F. ) ;
#27154 = ADVANCED_FACE ( 'NONE', ( #17783 ), #1712, .T. ) ;
#27155 = CYLINDRICAL_SURFACE ( 'NONE', #11253, 5.000000000000004441 ) ;
#27156 = AXIS2_PLACEMENT_3D ( 'NONE', #12150, #22636, #16033 ) ;
#27157 = DIRECTION ( 'NONE',  ( 0.000000000000000000, -1.000000000000000000, 0.000000000000000000 ) ) ;
#27158 = CARTESIAN_POINT ( 'NONE',  ( -215.6254804987312070, 60.26473849368080948, -13.41209097273894457 ) ) ;
#27159=STYLED_ITEM('',(#28434),#8800);
#27160 = FACE_OUTER_BOUND ( 'NONE', #1307, .T. ) ;
#27161 = DIRECTION ( 'NONE',  ( 0.4528218681374320820, 0.8916010070297846202, -0.000000000000000000 ) ) ;
#27162 = CARTESIAN_POINT ( 'NONE',  ( 157.4999999999998579, 138.4940622560211239, 45.00000000000000000 ) ) ;
#27163 = LINE ( 'NONE', #25681, #22219 ) ;
#27164 = VERTEX_POINT ( 'NONE', #5140 ) ;
#27165 = DIRECTION ( 'NONE',  ( 0.5555587585212683477, 0.8314772792026894344, -0.000000000000000000 ) ) ;
#27166 = CARTESIAN_POINT ( 'NONE',  ( -231.0952835391969415, 75.72709865442921284, 15.86948571459985047 ) ) ;
#27167 = DIRECTION ( 'NONE',  ( -0.000000000000000000, -0.000000000000000000, -1.000000000000000000 ) ) ;
#27168 = ORIENTED_EDGE ( 'NONE', *, *, #1380, .T. ) ;
#27169 = DIRECTION ( 'NONE',  ( 0.000000000000000000, 0.000000000000000000, 1.000000000000000000 ) ) ;
#27170 = ORIENTED_EDGE ( 'NONE', *, *, #26039, .T. ) ;
#27171 = AXIS2_PLACEMENT_3D ( 'NONE', #18470, #3084, #12014 ) ;
#27172 = VECTOR ( 'NONE', #15240, 1000.000000000000000 ) ;
#27173 = CARTESIAN_POINT ( 'NONE',  ( 82.68942924499303615, 110.0997128786253683, 70.07812500014873081 ) ) ;
#27174 = CARTESIAN_POINT ( 'NONE',  ( 79.99999999999990052, 140.0000000000000000, 15.00000000000000000 ) ) ;
#27175 = ORIENTED_EDGE ( 'NONE', *, *, #6111, .T. ) ;
#27176 = AXIS2_PLACEMENT_3D ( 'NONE', #9058, #2291, #156 ) ;
#27177 = ORIENTED_EDGE ( 'NONE', *, *, #19928, .F. ) ;
#27178 = DIRECTION ( 'NONE',  ( 1.000000000000000000, 0.000000000000000000, 0.000000000000000000 ) ) ;
#27179 = AXIS2_PLACEMENT_3D ( 'NONE', #4875, #26711, #12989 ) ;
#27180 = DIRECTION ( 'NONE',  ( 1.000000000000000000, 0.000000000000000000, 0.000000000000000000 ) ) ;
#27181 = CARTESIAN_POINT ( 'NONE',  ( -210.0000000000000000, -212.3568517473289035, -89.99999999999990052 ) ) ;
#27182 = ORIENTED_EDGE ( 'NONE', *, *, #7852, .F. ) ;
#27183 = DIRECTION ( 'NONE',  ( 0.000000000000000000, -1.000000000000000000, 0.000000000000000000 ) ) ;
#27184 = VERTEX_POINT ( 'NONE', #9319 ) ;
#27185 = PLANE ( 'NONE',  #9324 ) ;
#27186 = EDGE_CURVE ( 'NONE', #1602, #25624, #18081, .T. ) ;
#27187 = EDGE_CURVE ( 'NONE', #23117, #28088, #26837, .T. ) ;
#27188 = CARTESIAN_POINT ( 'NONE',  ( -279.3160071107327553, -91.18033988749901653, 0.000000000000000000 ) ) ;
#27189 = PLANE ( 'NONE',  #11230 ) ;
#27190 = CARTESIAN_POINT ( 'NONE',  ( -4.592061942444369826, 132.3627631488751604, -15.98545474231262098 ) ) ;
#27191 = DIRECTION ( 'NONE',  ( 1.000000000000000000, 0.000000000000000000, -0.000000000000000000 ) ) ;
#27192 = AXIS2_PLACEMENT_3D ( 'NONE', #16635, #16221, #25246 ) ;
#27193 = CARTESIAN_POINT ( 'NONE',  ( 217.4999999999996305, 494.4107529906318632, -100.0000000000000142 ) ) ;
#27194 = CARTESIAN_POINT ( 'NONE',  ( 162.6191355986925373, 208.2828629619915830, -140.2311020877163799 ) ) ;
#27195 = ORIENTED_EDGE ( 'NONE', *, *, #22299, .F. ) ;
#27196 = TOROIDAL_SURFACE ( 'NONE', #7919, 66.76834224489934400, 2.000000000000000000 ) ;
#27197 = DIRECTION ( 'NONE',  ( -0.8916010070298049373, 0.4528218681373921140, 0.000000000000000000 ) ) ;
#27198 = DIRECTION ( 'NONE',  ( 0.000000000000000000, -1.000000000000000000, -0.000000000000000000 ) ) ;
#27199 = AXIS2_PLACEMENT_3D ( 'NONE', #427, #18097, #11499 ) ;
#27200 = LINE ( 'NONE', #7537, #1550 ) ;
#27201 = ORIENTED_EDGE ( 'NONE', *, *, #21835, .F. ) ;
#27202 = DIRECTION ( 'NONE',  ( 1.224646799147353207E-16, 1.000000000000000000, -0.000000000000000000 ) ) ;
#27203 = VECTOR ( 'NONE', #18907, 1000.000000000000000 ) ;
#27204 = VERTEX_POINT ( 'NONE', #8888 ) ;
#27205 = CARTESIAN_POINT ( 'NONE',  ( 146.9844428835009467, 225.6878133005969858, -45.00000000000000000 ) ) ;
#27206 = CARTESIAN_POINT ( 'NONE',  ( -210.0000000000000568, -220.0000000000000853, -110.0000000000000284 ) ) ;
#27207 = CARTESIAN_POINT ( 'NONE',  ( 65.00000000000000000, -120.0000000000000995, -69.99999999999998579 ) ) ;
#27208 = ORIENTED_EDGE ( 'NONE', *, *, #10005, .T. ) ;
#27209 = CARTESIAN_POINT ( 'NONE',  ( 157.4999999999998579, 43.19481197075347723, 45.00000000000000000 ) ) ;
#27210 = ORIENTED_EDGE ( 'NONE', *, *, #11547, .T. ) ;
#27211 = DIRECTION ( 'NONE',  ( -0.8916010070293783896, 0.4528218681382319422, 0.000000000000000000 ) ) ;
#27212 = CARTESIAN_POINT ( 'NONE',  ( 102.1959223267361239, 244.1336238956074851, 16.70134980617025633 ) ) ;
#27213 = ORIENTED_EDGE ( 'NONE', *, *, #27346, .T. ) ;
#27214 = VECTOR ( 'NONE', #22747, 1000.000000000000000 ) ;
#27215 = VERTEX_POINT ( 'NONE', #2839 ) ;
#27216 = CARTESIAN_POINT ( 'NONE',  ( 158.0000000000014779, 63.51174953456337136, 45.00000000000000000 ) ) ;
#27217 = VERTEX_POINT ( 'NONE', #22098 ) ;
#27218 = EDGE_CURVE ( 'NONE', #3825, #10815, #23277, .T. ) ;
#27219 = ORIENTED_EDGE ( 'NONE', *, *, #16229, .F. ) ;
#27220 = EDGE_LOOP ( 'NONE', ( #8810, #20220, #9596, #444 ) ) ;
#27221 = AXIS2_PLACEMENT_3D ( 'NONE', #18757, #7983, #1233 ) ;
#27222 = CARTESIAN_POINT ( 'NONE',  ( 109.8801565119851205, 257.7417414023682340, 41.08725989918679034 ) ) ;
#27223 = EDGE_CURVE ( 'NONE', #24562, #3282, #22532, .T. ) ;
#27224 = FACE_OUTER_BOUND ( 'NONE', #6607, .T. ) ;
#27225 = DIRECTION ( 'NONE',  ( -0.8916010070293383105, -0.4528218681383106015, 0.000000000000000000 ) ) ;
#27226 = CARTESIAN_POINT ( 'NONE',  ( 158.0000000000000284, 203.9527499549551806, -45.00000000000000000 ) ) ;
#27227 = CARTESIAN_POINT ( 'NONE',  ( 157.9999999999998579, 221.0000000000000284, -45.00000000000000000 ) ) ;
#27228 = LINE ( 'NONE', #20909, #23512 ) ;
#27229 = EDGE_CURVE ( 'NONE', #23180, #8916, #11376, .T. ) ;
#27230 = DIRECTION ( 'NONE',  ( -0.000000000000000000, -0.000000000000000000, -1.000000000000000000 ) ) ;
#27231 = CARTESIAN_POINT ( 'NONE',  ( 157.9999999999999716, 208.9684999699701393, 45.00000000000000000 ) ) ;
#27232 = CARTESIAN_POINT ( 'NONE',  ( -236.8177751472017007, 82.33896643611701904, -15.00000000000000000 ) ) ;
#27233 = CARTESIAN_POINT ( 'NONE',  ( -203.1779787704217313, 93.05164332230201296, -15.00000000000000000 ) ) ;
#27234 = ORIENTED_EDGE ( 'NONE', *, *, #9623, .T. ) ;
#27235 = VECTOR ( 'NONE', #22851, 1000.000000000000114 ) ;
#27236 = CARTESIAN_POINT ( 'NONE',  ( 134.9999999999998579, 220.0000000000000284, -105.0000000000000284 ) ) ;
#27237 = CARTESIAN_POINT ( 'NONE',  ( 32.36067977499787673, 79.99999999999998579, 100.0000000000000142 ) ) ;
#27238 = DIRECTION ( 'NONE',  ( 0.8916010070294808632, 0.4528218681380302146, 0.000000000000000000 ) ) ;
#27239 = TOROIDAL_SURFACE ( 'NONE', #8429, 19.29759039828519818, 4.355764593064427537 ) ;
#27240 = ORIENTED_EDGE ( 'NONE', *, *, #23253, .T. ) ;
#27241 = EDGE_CURVE ( 'NONE', #22164, #18948, #14482, .T. ) ;
#27242 = CARTESIAN_POINT ( 'NONE',  ( 157.4999999999998579, 108.3995621659365867, 45.00000000000000000 ) ) ;
#27243 = ORIENTED_EDGE ( 'NONE', *, *, #2274, .F. ) ;
#27244 = DIRECTION ( 'NONE',  ( 1.000000000000000000, 0.000000000000000000, 0.000000000000000000 ) ) ;
#27245 = ORIENTED_EDGE ( 'NONE', *, *, #22541, .F. ) ;
#27246 = ADVANCED_FACE ( 'NONE', ( #12050 ), #11912, .F. ) ;
#27247 = ORIENTED_EDGE ( 'NONE', *, *, #22662, .F. ) ;
#27248 = ORIENTED_EDGE ( 'NONE', *, *, #23941, .F. ) ;
#27249 = EDGE_LOOP ( 'NONE', ( #6926, #11394, #2261, #25568 ) ) ;
#27250 = CARTESIAN_POINT ( 'NONE',  ( -149.5572648096271848, 124.9576791546268311, 17.81785897815565534 ) ) ;
#27251 = TOROIDAL_SURFACE ( 'NONE', #5690, 14.95564396479129243, 3.532530335305412716 ) ;
#27252 = DIRECTION ( 'NONE',  ( -0.000000000000000000, -0.000000000000000000, -1.000000000000000000 ) ) ;
#27253 = CYLINDRICAL_SURFACE ( 'NONE', #8373, 30.00000000000000000 ) ;
#27254 = CARTESIAN_POINT ( 'NONE',  ( -47.91567955387318989, 130.8829598292664969, -16.39210129961528040 ) ) ;
#27255 = VECTOR ( 'NONE', #4901, 999.9999999999998863 ) ;
#27256 = CARTESIAN_POINT ( 'NONE',  ( -13.76394398213074766, 130.8819511421725963, 14.96772766278609090 ) ) ;
#27257 = FACE_OUTER_BOUND ( 'NONE', #20824, .T. ) ;
#27258 = DIRECTION ( 'NONE',  ( -0.8916010070296936929, -0.4528218681376112165, 0.000000000000000000 ) ) ;
#27259 = CARTESIAN_POINT ( 'NONE',  ( -127.8584414339096185, 131.6633539443355687, -14.66583002116424517 ) ) ;
#27260 = ADVANCED_FACE ( 'NONE', ( #1254 ), #23749, .T. ) ;
#27261 = ADVANCED_FACE ( 'NONE', ( #3114 ), #20935, .T. ) ;
#27262 = LINE ( 'NONE', #7599, #19999 ) ;
#27263 = CARTESIAN_POINT ( 'NONE',  ( -205.2934542684511712, 91.43051335233271004, -27.40145609480763156 ) ) ;
#27264 = DIRECTION ( 'NONE',  ( 1.000000000000000000, 0.000000000000000000, -0.000000000000000000 ) ) ;
#27265 = DIRECTION ( 'NONE',  ( 1.000000000000000000, -0.000000000000000000, -0.000000000000000000 ) ) ;
#27266 = LINE ( 'NONE', #19077, #13943 ) ;
#27267 = DIRECTION ( 'NONE',  ( -0.000000000000000000, -0.000000000000000000, -1.000000000000000000 ) ) ;
#27268 = CARTESIAN_POINT ( 'NONE',  ( 89.77759941121082932, 81.13568025369244197, -100.0000000000000142 ) ) ;
#27269 = PLANE ( 'NONE',  #2414 ) ;
#27271 = EDGE_LOOP ( 'NONE', ( #19316, #12488, #11450, #6479 ) ) ;
#27270 = VERTEX_POINT ( 'NONE', #5564 ) ;
#27272 = VECTOR ( 'NONE', #19842, 1000.000000000000000 ) ;
#27273 = EDGE_CURVE ( 'NONE', #18153, #27001, #12195, .T. ) ;
#27274 = ADVANCED_FACE ( 'NONE', ( #27386 ), #23098, .F. ) ;
#27275 = LINE ( 'NONE', #18663, #17540 ) ;
#27276 = ORIENTED_EDGE ( 'NONE', *, *, #9846, .T. ) ;
#27277 = VECTOR ( 'NONE', #15923, 1000.000000000000000 ) ;
#27279 = EDGE_CURVE ( 'NONE', #25901, #6688, #16774, .T. ) ;
#27278 = ORIENTED_EDGE ( 'NONE', *, *, #7316, .F. ) ;
#27280 = VERTEX_POINT ( 'NONE', #5285 ) ;
#27281 = EDGE_CURVE ( 'NONE', #6349, #13016, #22816, .T. ) ;
#27282 = EDGE_LOOP ( 'NONE', ( #27688, #13303, #22978, #6759 ) ) ;
#27283 = FACE_OUTER_BOUND ( 'NONE', #13633, .T. ) ;
#27284 = DIRECTION ( 'NONE',  ( -0.000000000000000000, -0.000000000000000000, -1.000000000000000000 ) ) ;
#27285 = DIRECTION ( 'NONE',  ( -0.8916010070299172918, -0.4528218681371710685, 0.000000000000000000 ) ) ;
#27286 = AXIS2_PLACEMENT_3D ( 'NONE', #20411, #7629, #875 ) ;
#27287 = CARTESIAN_POINT ( 'NONE',  ( 157.4999999999994884, 211.2224374737238577, 45.00000000000000000 ) ) ;
#27288 = LINE ( 'NONE', #7628, #474 ) ;
#27289 = CARTESIAN_POINT ( 'NONE',  ( 157.4999999999996305, 283.9508126914284958, 45.00000000000000000 ) ) ;
#27290 = VECTOR ( 'NONE', #21018, 1000.000000000000000 ) ;
#27291 = FACE_OUTER_BOUND ( 'NONE', #4772, .T. ) ;
#27292 = CARTESIAN_POINT ( 'NONE',  ( -212.6433224921749456, 72.57850140501174963, -29.69533576542902154 ) ) ;
#27293 = CARTESIAN_POINT ( 'NONE',  ( 112.3374974218580320, 200.3420669299287340, -146.9347961558894156 ) ) ;
#27294 = LINE ( 'NONE', #7908, #14279 ) ;
#27295 = CYLINDRICAL_SURFACE ( 'NONE', #13898, 22.49999999999999289 ) ;
#27296 = CARTESIAN_POINT ( 'NONE',  ( 157.9999999999996589, 276.6811251726610976, 45.00000000000000000 ) ) ;
#27297 = VERTEX_POINT ( 'NONE', #20794 ) ;
#27298 = CARTESIAN_POINT ( 'NONE',  ( 158.0000000000010800, 101.1298746471690038, -45.00000000000000000 ) ) ;
#27299 = FACE_OUTER_BOUND ( 'NONE', #6118, .T. ) ;
#27300 = CARTESIAN_POINT ( 'NONE',  ( 157.4999999999998579, 168.5885623461056184, 45.00000000000000000 ) ) ;
#27301 = ORIENTED_EDGE ( 'NONE', *, *, #7852, .T. ) ;
#27302 = DIRECTION ( 'NONE',  ( 0.000000000000000000, 0.000000000000000000, 1.000000000000000000 ) ) ;
#27304 = ORIENTED_EDGE ( 'NONE', *, *, #2140, .T. ) ;
#27303 = EDGE_CURVE ( 'NONE', #8771, #20071, #5418, .T. ) ;
#27305 = AXIS2_PLACEMENT_3D ( 'NONE', #10294, #25651, #14471 ) ;
#27306 = EDGE_CURVE ( 'NONE', #12327, #11955, #14201, .T. ) ;
#27307 = CARTESIAN_POINT ( 'NONE',  ( 158.0000000000014211, 68.52749954957745615, 45.00000000000000000 ) ) ;
#27308 = LINE ( 'NONE', #23431, #14962 ) ;
#27309 = ORIENTED_EDGE ( 'NONE', *, *, #24046, .F. ) ;
#27310 = VECTOR ( 'NONE', #23910, 1000.000000000000000 ) ;
#27311 = VERTEX_POINT ( 'NONE', #25389 ) ;
#27312 = CARTESIAN_POINT ( 'NONE',  ( 82.68942924499074820, 110.0997128786250840, -70.07812500014861712 ) ) ;
#27313 = CARTESIAN_POINT ( 'NONE',  ( 157.9999999999997442, 253.6023750975910502, 45.00000000000000000 ) ) ;
#27314 = DIRECTION ( 'NONE',  ( -0.000000000000000000, 0.000000000000000000, -1.000000000000000000 ) ) ;
#27315 = ORIENTED_EDGE ( 'NONE', *, *, #23582, .F. ) ;
#27316 = DIRECTION ( 'NONE',  ( -1.000000000000000000, 0.000000000000000000, 0.000000000000000000 ) ) ;
#27317 = VERTEX_POINT ( 'NONE', #20512 ) ;
#27318 = DIRECTION ( 'NONE',  ( -0.000000000000000000, -0.000000000000000000, -1.000000000000000000 ) ) ;
#27319 = CARTESIAN_POINT ( 'NONE',  ( 157.4999999999998579, 50.71843699327460797, -45.00000000000000000 ) ) ;
#27320 = PLANE ( 'NONE',  #23609 ) ;
#27321 = CARTESIAN_POINT ( 'NONE',  ( -38.50748414645865125, 128.7743013786471238, -17.17767432558748908 ) ) ;
#27322 = AXIS2_PLACEMENT_3D ( 'NONE', #21643, #17469, #4673 ) ;
#27323 = CARTESIAN_POINT ( 'NONE',  ( 158.0000000000003411, 173.8582498648732440, 45.00000000000000000 ) ) ;
#27324 = AXIS2_PLACEMENT_3D ( 'NONE', #3461, #1032, #1312 ) ;
#27325 = CARTESIAN_POINT ( 'NONE',  ( -207.5044420441007276, 75.59897387903043864, -45.00000000000000000 ) ) ;
#27326 = LINE ( 'NONE', #24908, #22163 ) ;
#27327 = VERTEX_POINT ( 'NONE', #18507 ) ;
#27328 = EDGE_CURVE ( 'NONE', #991, #21625, #3684, .T. ) ;
#27329 = CARTESIAN_POINT ( 'NONE',  ( -210.0000000000000568, -152.0000000000000284, -94.99999999999987210 ) ) ;
#27330 = TOROIDAL_SURFACE ( 'NONE', #3486, 33.76444293738737912, 9.999999999999996447 ) ;
#27331 = LINE ( 'NONE', #7246, #16164 ) ;
#27332 = CARTESIAN_POINT ( 'NONE',  ( 116.5224093497742786, 212.3463313526978595, 45.00000000000000000 ) ) ;
#27333 = ORIENTED_EDGE ( 'NONE', *, *, #8385, .T. ) ;
#27334 = CARTESIAN_POINT ( 'NONE',  ( 157.9999999999997726, 246.5866250825770294, 45.00000000000000000 ) ) ;
#27335 = ORIENTED_EDGE ( 'NONE', *, *, #27000, .T. ) ;
#27336 = CARTESIAN_POINT ( 'NONE',  ( 267.4999999999996021, 194.4107529906318064, 100.0000000000000284 ) ) ;
#27337 = CARTESIAN_POINT ( 'NONE',  ( -141.6428522700808230, 17.24192588826928585, 83.00000000000001421 ) ) ;
#27338 = CARTESIAN_POINT ( 'NONE',  ( -260.0000000000001137, -157.0000000000000284, -59.99999999999986500 ) ) ;
#27339 = EDGE_LOOP ( 'NONE', ( #1831, #11063, #22557, #12075 ) ) ;
#27340 = CYLINDRICAL_SURFACE ( 'NONE', #16145, 5.999999999999991118 ) ;
#27341 = EDGE_CURVE ( 'NONE', #17217, #18102, #22954, .T. ) ;
#27342 = VERTEX_POINT ( 'NONE', #5709 ) ;
#27343 = EDGE_CURVE ( 'NONE', #17857, #4054, #6385, .T. ) ;
#27344 = ADVANCED_FACE ( 'NONE', ( #25245 ), #12333, .F. ) ;
#27345 = CARTESIAN_POINT ( 'NONE',  ( -127.2554728363764696, 130.3923307403294416, 16.55011143430600740 ) ) ;
#27346 = EDGE_CURVE ( 'NONE', #12421, #378, #27667, .T. ) ;
#27347 = CARTESIAN_POINT ( 'NONE',  ( 107.4212975031135642, 250.1603648754377502, 27.81198034436183164 ) ) ;
#27348 = ORIENTED_EDGE ( 'NONE', *, *, #17194, .T. ) ;
#27349 = VECTOR ( 'NONE', #28292, 1000.000000000000114 ) ;
#27350 = EDGE_LOOP ( 'NONE', ( #9138, #9845, #2498, #12884 ) ) ;
#27351 = DIRECTION ( 'NONE',  ( 1.000000000000000000, 0.000000000000000000, -0.000000000000000000 ) ) ;
#27352 = ORIENTED_EDGE ( 'NONE', *, *, #4436, .F. ) ;
#27353 = ORIENTED_EDGE ( 'NONE', *, *, #23621, .F. ) ;
#27354 = VECTOR ( 'NONE', #26814, 999.9999999999998863 ) ;
#27355 = ORIENTED_EDGE ( 'NONE', *, *, #3596, .F. ) ;
#27356 = CARTESIAN_POINT ( 'NONE',  ( 109.4601507141017009, 253.2495769758999984, 39.14599534723758012 ) ) ;
#27357 = CARTESIAN_POINT ( 'NONE',  ( 157.4999999999998579, 191.1594374136689964, 45.00000000000000000 ) ) ;
#27358 = DIRECTION ( 'NONE',  ( -0.000000000000000000, -0.000000000000000000, 1.000000000000000000 ) ) ;
#27359 = CARTESIAN_POINT ( 'NONE',  ( 158.0000000000005400, 158.3031248123239436, 45.00000000000000000 ) ) ;
#27360 = CARTESIAN_POINT ( 'NONE',  ( 232.4999999999996305, 133.0668745871126930, -36.86484227207694886 ) ) ;
#27361 = DIRECTION ( 'NONE',  ( -0.000000000000000000, -0.000000000000000000, -1.000000000000000000 ) ) ;
#27362 = CARTESIAN_POINT ( 'NONE',  ( 124.9999999999998579, 220.0000000000000284, 99.00000000000001421 ) ) ;
#27363 = CARTESIAN_POINT ( 'NONE',  ( 187.4999999999996305, 526.4263741777961059, 74.99999999999995737 ) ) ;
#27364 = FACE_OUTER_BOUND ( 'NONE', #21526, .T. ) ;
#27365 = LINE ( 'NONE', #7574, #23108 ) ;
#27366 = EDGE_LOOP ( 'NONE', ( #14262, #27195, #3136, #15594 ) ) ;
#27367 = EDGE_CURVE ( 'NONE', #21137, #620, #836, .T. ) ;
#27368 = EDGE_CURVE ( 'NONE', #25995, #17824, #15047, .T. ) ;
#27369 = CARTESIAN_POINT ( 'NONE',  ( 108.2137533302215360, 251.6609783837992040, -30.47578649309999577 ) ) ;
#27370 = CARTESIAN_POINT ( 'NONE',  ( 157.4999999999998579, 43.19481197075347723, -45.00000000000000000 ) ) ;
#27371 = CARTESIAN_POINT ( 'NONE',  ( 33.10302365956999182, 203.2034914284457159, -13.00000000000000000 ) ) ;
#27372 = FACE_OUTER_BOUND ( 'NONE', #25028, .T. ) ;
#27373 = EDGE_LOOP ( 'NONE', ( #17134, #26439, #8282, #25237, #12158 ) ) ;
#27374 = DIRECTION ( 'NONE',  ( 1.049727191138617093E-16, 0.5150380749100560429, -0.8571673007021111124 ) ) ;
#27375 = VERTEX_POINT ( 'NONE', #6268 ) ;
#27376 = EDGE_CURVE ( 'NONE', #24118, #14154, #8238, .T. ) ;
#27377 = CARTESIAN_POINT ( 'NONE',  ( 2.399999999999999911, -1.249999999999998890, -8.000000000000000000 ) ) ;
#27378 = ORIENTED_EDGE ( 'NONE', *, *, #6567, .T. ) ;
#27379 = ORIENTED_EDGE ( 'NONE', *, *, #15112, .T. ) ;
#27380 = ADVANCED_FACE ( 'NONE', ( #1675, #8146 ), #15044, .T. ) ;
#27381 = EDGE_LOOP ( 'NONE', ( #25828, #1587, #4370, #10225 ) ) ;
#27382 = ORIENTED_EDGE ( 'NONE', *, *, #24971, .T. ) ;
#27383 = ORIENTED_EDGE ( 'NONE', *, *, #21453, .F. ) ;
#27384 = CARTESIAN_POINT ( 'NONE',  ( -82.71680601032872460, 136.4209726650630330, 13.49001633003910960 ) ) ;
#27385 = VECTOR ( 'NONE', #12364, 1000.000000000000000 ) ;
#27386 = FACE_OUTER_BOUND ( 'NONE', #2622, .T. ) ;
#27387 = CARTESIAN_POINT ( 'NONE',  ( -211.1943141956539876, -220.0000000000000853, -91.97569866068964473 ) ) ;
#27388 = CARTESIAN_POINT ( 'NONE',  ( -77.56758787812782430, 136.3063890311531736, -15.17881120916173110 ) ) ;
#27389 = CARTESIAN_POINT ( 'NONE',  ( -1.260211142396240103, 135.5645450900976527, 13.59434970638475804 ) ) ;
#27390 = CARTESIAN_POINT ( 'NONE',  ( -214.2457779686714900, 55.07866962813993439, 44.91461755630199804 ) ) ;
#27391 = CARTESIAN_POINT ( 'NONE',  ( 158.0000000000015348, 60.49599951954928656, 45.00000000000000000 ) ) ;
#27392 = DIRECTION ( 'NONE',  ( 0.4528218681375107413, -0.8916010070297447632, 0.000000000000000000 ) ) ;
#27393 = LINE ( 'NONE', #14213, #28254 ) ;
#27394 = DIRECTION ( 'NONE',  ( -0.8916010070293383105, -0.4528218681383106015, 0.000000000000000000 ) ) ;
#27395 = PLANE ( 'NONE',  #24691 ) ;
#27396 = CYLINDRICAL_SURFACE ( 'NONE', #159, 5.999999999999991118 ) ;
#27397 = VERTEX_POINT ( 'NONE', #25662 ) ;
#27398 = AXIS2_PLACEMENT_3D ( 'NONE', #22286, #7630, #9509 ) ;
#27399 = EDGE_CURVE ( 'NONE', #3490, #13244, #1952, .T. ) ;
#27400 = LINE ( 'NONE', #25262, #2721 ) ;
#27401 = CARTESIAN_POINT ( 'NONE',  ( 144.9999999999998863, 220.0000000000000284, -90.00000000000002842 ) ) ;
#27402 = LINE ( 'NONE', #4092, #3793 ) ;
#27404 = VERTEX_POINT ( 'NONE', #14907 ) ;
#27403 = ORIENTED_EDGE ( 'NONE', *, *, #20136, .F. ) ;
#27405 = AXIS2_PLACEMENT_3D ( 'NONE', #10164, #23372, #7449 ) ;
#27406 = CIRCLE ( 'NONE', #3089, 414.0408555545579929 ) ;
#27407 = FACE_OUTER_BOUND ( 'NONE', #7725, .T. ) ;
#27408 = ORIENTED_EDGE ( 'NONE', *, *, #16572, .T. ) ;
#27409 = ORIENTED_EDGE ( 'NONE', *, *, #5590, .T. ) ;
#27410 = VERTEX_POINT ( 'NONE', #28232 ) ;
#27411 = EDGE_CURVE ( 'NONE', #23124, #20650, #9621, .T. ) ;
#27412 = EDGE_CURVE ( 'NONE', #16446, #7676, #3828, .T. ) ;
#27413 = ORIENTED_EDGE ( 'NONE', *, *, #3228, .T. ) ;
#27414 = VERTEX_POINT ( 'NONE', #8713 ) ;
#27415 = DIRECTION ( 'NONE',  ( 0.8916010070294909662, 0.4528218681380102306, 0.000000000000000000 ) ) ;
#27416 = FACE_OUTER_BOUND ( 'NONE', #27737, .T. ) ;
#27417 = AXIS2_PLACEMENT_3D ( 'NONE', #16508, #27265, #7602 ) ;
#27418 = VECTOR ( 'NONE', #3485, 1000.000000000000000 ) ;
#27419 = PLANE ( 'NONE',  #25648 ) ;
#27420 = LINE ( 'NONE', #28269, #167 ) ;
#27421 = EDGE_CURVE ( 'NONE', #13840, #8625, #23660, .T. ) ;
#27422 = CARTESIAN_POINT ( 'NONE',  ( -68.57415822541635464, -18.01420295945611727, 100.0000000000000000 ) ) ;
#27423 = EDGE_CURVE ( 'NONE', #4484, #11107, #5986, .T. ) ;
#27424 = CARTESIAN_POINT ( 'NONE',  ( 64.99999999999998579, -173.6051637141654567, -69.99999999999998579 ) ) ;
#27425 = DIRECTION ( 'NONE',  ( -0.000000000000000000, 0.000000000000000000, -1.000000000000000000 ) ) ;
#27426 = CARTESIAN_POINT ( 'NONE',  ( -214.1728591254723142, 55.16903133821739402, -44.30008786503535845 ) ) ;
#27428 = CARTESIAN_POINT ( 'NONE',  ( 179.9999999999999147, 330.0000000000000000, 100.0000000000000142 ) ) ;
#27427 = MECHANICAL_DESIGN_GEOMETRIC_PRESENTATION_REPRESENTATION (  '', ( #21535 ), #6861 ) ;
#27429 = DIRECTION ( 'NONE',  ( -0.8916010070298766577, -0.4528218681372509491, 0.000000000000000000 ) ) ;
#27430 = CARTESIAN_POINT ( 'NONE',  ( 157.4999999999998579, 78.30506207585207790, -45.00000000000000000 ) ) ;
#27431 = CARTESIAN_POINT ( 'NONE',  ( 154.4185842870420799, 207.6339745962155803, 45.00000000000000000 ) ) ;
#27432 = ORIENTED_EDGE ( 'NONE', *, *, #23729, .T. ) ;
#27433 = CARTESIAN_POINT ( 'NONE',  ( 157.9999999999998863, 218.4921249924925348, -45.00000000000000000 ) ) ;
#27434 = AXIS2_PLACEMENT_3D ( 'NONE', #18618, #1513, #20913 ) ;
#27435 = VECTOR ( 'NONE', #10172, 1000.000000000000227 ) ;
#27436 = DIRECTION ( 'NONE',  ( -0.9711705445023439687, 0.2383857661250367854, 0.000000000000000000 ) ) ;
#27437 = ORIENTED_EDGE ( 'NONE', *, *, #148, .F. ) ;
#27438 = DIRECTION ( 'NONE',  ( 1.000000000000000000, 0.000000000000000000, 0.000000000000000000 ) ) ;
#27439 = ORIENTED_EDGE ( 'NONE', *, *, #22946, .T. ) ;
#27440 = VERTEX_POINT ( 'NONE', #6555 ) ;
#27441 = EDGE_CURVE ( 'NONE', #1982, #9667, #21214, .T. ) ;
#27442 = CARTESIAN_POINT ( 'NONE',  ( -227.8378063125350366, 130.6400894613935577, -13.00000000000000178 ) ) ;
#27443 = CARTESIAN_POINT ( 'NONE',  ( 79.99999999999991473, 140.0000000000000000, 45.00000000000000000 ) ) ;
#27444 = ORIENTED_EDGE ( 'NONE', *, *, #26220, .T. ) ;
#27445 = EDGE_LOOP ( 'NONE', ( #9568, #14637, #26152 ) ) ;
#27446 = CARTESIAN_POINT ( 'NONE',  ( 85.90765579575543143, 110.5723347142871091, -70.58593750016461854 ) ) ;
#27447 = CARTESIAN_POINT ( 'NONE',  ( 109.5123478387949234, 253.5801691942621403, 39.43342786172818393 ) ) ;
#27448 = VECTOR ( 'NONE', #12313, 1000.000000000000000 ) ;
#27449 = FACE_OUTER_BOUND ( 'NONE', #7587, .T. ) ;
#27450 = ORIENTED_EDGE ( 'NONE', *, *, #10194, .F. ) ;
#27451 = CARTESIAN_POINT ( 'NONE',  ( -230.8465493730670346, 92.52399884504492888, 12.99999999980437160 ) ) ;
#27452 = ORIENTED_EDGE ( 'NONE', *, *, #13849, .F. ) ;
#27453 = CARTESIAN_POINT ( 'NONE',  ( 157.9999999999997726, 244.0787500750700474, -45.00000000000000000 ) ) ;
#27454 = VECTOR ( 'NONE', #27059, 1000.000000000000000 ) ;
#27455 = AXIS2_PLACEMENT_3D ( 'NONE', #17979, #26734, #15842 ) ;
#27456 = CARTESIAN_POINT ( 'NONE',  ( 140.5127944162910865, 243.3752990424897575, 45.00000000000000000 ) ) ;
#27457 = LINE ( 'NONE', #25177, #11693 ) ;
#27458 = CARTESIAN_POINT ( 'NONE',  ( -40.48090269740500702, 130.4480578055027706, -16.52329147365227868 ) ) ;
#27459 = DIRECTION ( 'NONE',  ( -1.000000000000000000, 1.850371707708594366E-15, 0.000000000000000000 ) ) ;
#27460 = EDGE_CURVE ( 'NONE', #10156, #23257, #12615, .T. ) ;
#27461 = ADVANCED_FACE ( 'NONE', ( #767 ), #20156, .F. ) ;
#27462 = FACE_OUTER_BOUND ( 'NONE', #28079, .T. ) ;
#27463 = CARTESIAN_POINT ( 'NONE',  ( -200.0139728499287060, 95.39988079771768525, -31.09496554298159765 ) ) ;
#27464 = ORIENTED_EDGE ( 'NONE', *, *, #20047, .F. ) ;
#27465 = CARTESIAN_POINT ( 'NONE',  ( 134.9999999999998579, -327.2004514666934369, 84.99999999999995737 ) ) ;
#27466 = ADVANCED_FACE ( 'NONE', ( #9243 ), #22745, .F. ) ;
#27467 = CARTESIAN_POINT ( 'NONE',  ( 134.9999999999998579, 220.0000000000000284, -100.0000000000000142 ) ) ;
#27468 = DIRECTION ( 'NONE',  ( -0.000000000000000000, -0.000000000000000000, -1.000000000000000000 ) ) ;
#27469 = LINE ( 'NONE', #11716, #11191 ) ;
#27470 = VERTEX_POINT ( 'NONE', #25040 ) ;
#27471 = CARTESIAN_POINT ( 'NONE',  ( 116.8899838958982400, 233.3643110186103229, 99.51050955275449894 ) ) ;
#27472 = VERTEX_POINT ( 'NONE', #9533 ) ;
#27473 = CIRCLE ( 'NONE', #10986, 8.000000000000000000 ) ;
#27474 = LINE ( 'NONE', #7814, #2437 ) ;
#27475 = CARTESIAN_POINT ( 'NONE',  ( 69.99612328191057031, 261.2290884209365345, 45.00000000000000000 ) ) ;
#27476 = DIRECTION ( 'NONE',  ( -0.000000000000000000, 1.000000000000000000, -1.387778780781445429E-16 ) ) ;
#27477 = VERTEX_POINT ( 'NONE', #20298 ) ;
#27478 = LINE ( 'NONE', #9835, #10169 ) ;
#27479 = CIRCLE ( 'NONE', #14655, 50.00000000000000711 ) ;
#27480 = LINE ( 'NONE', #19151, #9288 ) ;
#27481 = VERTEX_POINT ( 'NONE', #22879 ) ;
#27482 = VECTOR ( 'NONE', #27267, 1000.000000000000000 ) ;
#27483 = DIRECTION ( 'NONE',  ( 1.000000000000000000, 1.541976423090495880E-16, 0.000000000000000000 ) ) ;
#27484 = LINE ( 'NONE', #14575, #23675 ) ;
#27485 = VERTEX_POINT ( 'NONE', #9393 ) ;
#27486 = EDGE_LOOP ( 'NONE', ( #9087, #25517, #19941, #22263 ) ) ;
#27487 = AXIS2_PLACEMENT_3D ( 'NONE', #20684, #1004, #27558 ) ;
#27488 = LINE ( 'NONE', #12155, #23708 ) ;
#27489 = ORIENTED_EDGE ( 'NONE', *, *, #13000, .F. ) ;
#27490 = ORIENTED_EDGE ( 'NONE', *, *, #24991, .F. ) ;
#27491 = VERTEX_POINT ( 'NONE', #22314 ) ;
#27492 = CARTESIAN_POINT ( 'NONE',  ( 109.5201339680880324, 255.4997179839102444, 37.19466046298244777 ) ) ;
#27493 = AXIS2_PLACEMENT_3D ( 'NONE', #4259, #19492, #15339 ) ;
#27494 = FACE_OUTER_BOUND ( 'NONE', #6969, .T. ) ;
#27495 = ADVANCED_FACE ( 'NONE', ( #16005 ), #18429, .F. ) ;
#27496 = DIRECTION ( 'NONE',  ( 1.000000000000000000, -0.000000000000000000, -0.000000000000000000 ) ) ;
#27497 = CIRCLE ( 'NONE', #16072, 6.025000000000002132 ) ;
#27498 = EDGE_CURVE ( 'NONE', #17489, #226, #24613, .T. ) ;
#27499 = CARTESIAN_POINT ( 'NONE',  ( 158.0000000000006821, 140.7479997597746433, 45.00000000000000000 ) ) ;
#27500 = CIRCLE ( 'NONE', #11016, 60.00000000000001421 ) ;
#27501 = CARTESIAN_POINT ( 'NONE',  ( 134.9999999999998579, 220.0000000000000284, -100.0000000000000142 ) ) ;
#27502 = FACE_OUTER_BOUND ( 'NONE', #20706, .T. ) ;
#27503 = EDGE_CURVE ( 'NONE', #5099, #4881, #26763, .T. ) ;
#27504 = DIRECTION ( 'NONE',  ( 0.000000000000000000, -1.000000000000000000, 0.000000000000000000 ) ) ;
#27505 = CARTESIAN_POINT ( 'NONE',  ( -263.2377953986417651, -166.4145296663307647, 109.9218949472355291 ) ) ;
#27506 = CARTESIAN_POINT ( 'NONE',  ( 0.3651377028998192276, -1.249999999999998890, -7.402212548648222423 ) ) ;
#27507 = LINE ( 'NONE', #27233, #25841 ) ;
#27508 = ORIENTED_EDGE ( 'NONE', *, *, #1128, .F. ) ;
#27509 = CARTESIAN_POINT ( 'NONE',  ( -6.855911443193040355, 133.1088201606621624, 14.22081536340692942 ) ) ;
#27510 = CYLINDRICAL_SURFACE ( 'NONE', #9645, 22.49999999999999289 ) ;
#27511 = CARTESIAN_POINT ( 'NONE',  ( 146.9844428835009467, 225.6878133005969858, 45.00000000000000000 ) ) ;
#27512 = LINE ( 'NONE', #21198, #15074 ) ;
#27513 = CARTESIAN_POINT ( 'NONE',  ( -146.6428522700808230, 74.54464929955099706, 83.00000000000001421 ) ) ;
#27514 = VERTEX_POINT ( 'NONE', #9673 ) ;
#27515 = VECTOR ( 'NONE', #27225, 1000.000000000000114 ) ;
#27516 = LINE ( 'NONE', #14328, #1507 ) ;
#27517 = EDGE_LOOP ( 'NONE', ( #13202, #20752, #6190, #25074 ) ) ;
#27518 = CARTESIAN_POINT ( 'NONE',  ( 95.82124051657368113, -20.23615780638419182, 45.00000000000000000 ) ) ;
#27519 = VERTEX_POINT ( 'NONE', #24758 ) ;
#27520 = ORIENTED_EDGE ( 'NONE', *, *, #19271, .T. ) ;
#27521 = ORIENTED_EDGE ( 'NONE', *, *, #10141, .F. ) ;
#27522 = ORIENTED_EDGE ( 'NONE', *, *, #21568, .F. ) ;
#27523 = FACE_OUTER_BOUND ( 'NONE', #23126, .T. ) ;
#27524 = DIRECTION ( 'NONE',  ( 0.000000000000000000, -1.000000000000000000, 0.000000000000000000 ) ) ;
#27525 = CARTESIAN_POINT ( 'NONE',  ( 157.4999999999998579, 113.4153121809506786, 45.00000000000000000 ) ) ;
#27526 = EDGE_CURVE ( 'NONE', #19430, #19942, #14130, .T. ) ;
#27527 = CARTESIAN_POINT ( 'NONE',  ( 158.0000000000010516, 103.6377496546760568, 45.00000000000000000 ) ) ;
#27528 = EDGE_CURVE ( 'NONE', #23088, #8776, #21070, .T. ) ;
#27529 = CARTESIAN_POINT ( 'NONE',  ( -208.0231409554068875, 75.22252239880569391, 40.22632386312260167 ) ) ;
#27530 = DIRECTION ( 'NONE',  ( -0.000000000000000000, 0.000000000000000000, 1.000000000000000000 ) ) ;
#27531 = LINE ( 'NONE', #9613, #7164 ) ;
#27532 = CIRCLE ( 'NONE', #2770, 10.00000000000000888 ) ;
#27533 = ADVANCED_FACE ( 'NONE', ( #7234 ), #18007, .T. ) ;
#27534 = CARTESIAN_POINT ( 'NONE',  ( 130.4830771568834962, 249.6593242776497164, -141.0313312019551688 ) ) ;
#27535 = CARTESIAN_POINT ( 'NONE',  ( -214.1330451156402148, 86.77492310787303609, 22.28634443271844745 ) ) ;
#27536 = CARTESIAN_POINT ( 'NONE',  ( 157.9999999999997158, 258.6181251126050711, 45.00000000000000000 ) ) ;
#27537 = DIRECTION ( 'NONE',  ( 0.000000000000000000, 0.000000000000000000, -1.000000000000000000 ) ) ;
#27538 = CARTESIAN_POINT ( 'NONE',  ( 158.0000000000011084, 98.62199963966197913, -45.00000000000000000 ) ) ;
#27539 = ORIENTED_EDGE ( 'NONE', *, *, #16032, .F. ) ;
#27540 = AXIS2_PLACEMENT_3D ( 'NONE', #19924, #17766, #15349 ) ;
#27541 = DIRECTION ( 'NONE',  ( -0.9239321509641975627, -1.061807240666849658E-15, 0.3825563754725197496 ) ) ;
#27542 = CARTESIAN_POINT ( 'NONE',  ( -76.25760768171836901, 154.8982798170083299, -13.00000000000000000 ) ) ;
#27544 = VERTEX_POINT ( 'NONE', #18293 ) ;
#27543 = ORIENTED_EDGE ( 'NONE', *, *, #19187, .T. ) ;
#27545 = DIRECTION ( 'NONE',  ( -0.000000000000000000, -0.000000000000000000, -1.000000000000000000 ) ) ;
#27546 = ORIENTED_EDGE ( 'NONE', *, *, #26829, .T. ) ;
#27547 = ORIENTED_EDGE ( 'NONE', *, *, #25316, .T. ) ;
#27548 = ORIENTED_EDGE ( 'NONE', *, *, #25672, .F. ) ;
#27549 = AXIS2_PLACEMENT_3D ( 'NONE', #21290, #1609, #10379 ) ;
#27550 = ORIENTED_EDGE ( 'NONE', *, *, #11443, .T. ) ;
#27551 = EDGE_CURVE ( 'NONE', #25965, #12172, #904, .T. ) ;
#27552 = B_SPLINE_CURVE_WITH_KNOTS ( 'NONE', 3,
 ( #7735, #709, #16505, #14627, #27677, #23811, #3839, #4118, #27816, #14916, #12762, #27534, #3975, #17199, #21503, #12626, #25533, #1403, #10313, #25958, #21650, #1820, #16916, #7872, #23246, #5852, #8154, #21364, #3550, #10595, #6278, #19071, #19352, #12904, #12483, #23381, #1962, #17056, #28099, #21082, #8014, #8443 ),
 .UNSPECIFIED., .F., .F.,
 ( 4, 2, 2, 2, 2, 2, 2, 2, 2, 2, 2, 2, 2, 2, 2, 2, 2, 2, 2, 2, 4 ),
 ( 0.01880622955133632798, 0.01998131524074754292, 0.02115640093015875439, 0.02174394377486431329, 0.02233148661956986872, 0.02350657230898093447, 0.02468165799839200023, 0.02585674368780306598, 0.02644428653250857630, 0.02703182937721408663, 0.02820691506662520442, 0.02938200075603631875, 0.03055708644544743655, 0.03173217213485855087, 0.03231971497956409589, 0.03290725782426963397, 0.03408234351368061299, 0.03525742920309159201, 0.03584497204779707458, 0.03643251489250255715, 0.03760760058191346678 ),
 .UNSPECIFIED. ) ;
#27553 = ORIENTED_EDGE ( 'NONE', *, *, #23729, .F. ) ;
#27554 = ORIENTED_EDGE ( 'NONE', *, *, #27847, .F. ) ;
#27555 = LINE ( 'NONE', #22987, #11358 ) ;
#27556 = VECTOR ( 'NONE', #21692, 1000.000000000000000 ) ;
#27557 = ADVANCED_FACE ( 'NONE', ( #27044 ), #2914, .F. ) ;
#27558 = DIRECTION ( 'NONE',  ( 0.6140342761796242499, -0.7892793597178155984, 0.000000000000000000 ) ) ;
#27559 = LINE ( 'NONE', #27986, #28123 ) ;
#27560 = DIRECTION ( 'NONE',  ( -0.000000000000000000, -0.000000000000000000, 1.000000000000000000 ) ) ;
#27561 = EDGE_CURVE ( 'NONE', #268, #301, #27479, .T. ) ;
#27562 = DIRECTION ( 'NONE',  ( 0.000000000000000000, -1.000000000000000000, 0.000000000000000000 ) ) ;
#27563 = DIRECTION ( 'NONE',  ( -0.000000000000000000, 0.000000000000000000, -1.000000000000000000 ) ) ;
#27564 = DIRECTION ( 'NONE',  ( -0.000000000000000000, -0.000000000000000000, -1.000000000000000000 ) ) ;
#27565 = ADVANCED_FACE ( 'NONE', ( #13998 ), #1041, .F. ) ;
#27566 = CIRCLE ( 'NONE', #20692, 6.000000000000005329 ) ;
#27567 = CARTESIAN_POINT ( 'NONE',  ( 432.4999999999996589, 44.41075299063184190, 100.0000000000000426 ) ) ;
#27568 = CARTESIAN_POINT ( 'NONE',  ( 134.9999999999998579, 220.0000000000000284, -90.00000000000002842 ) ) ;
#27569 = LINE ( 'NONE', #14525, #1424 ) ;
#27570 = CARTESIAN_POINT ( 'NONE',  ( -277.2150368962633706, -237.2150368962634559, -94.99999999999985789 ) ) ;
#27571 = ORIENTED_EDGE ( 'NONE', *, *, #23057, .F. ) ;
#27572 = AXIS2_PLACEMENT_3D ( 'NONE', #14294, #10396, #12146 ) ;
#27573 = CARTESIAN_POINT ( 'NONE',  ( -195.0817138475443357, 99.65346455659198455, 32.12633496786403953 ) ) ;
#27574 = AXIS2_PLACEMENT_3D ( 'NONE', #6710, #24109, #15636 ) ;
#27575 = PLANE ( 'NONE',  #6220 ) ;
#27576 = ORIENTED_EDGE ( 'NONE', *, *, #18562, .F. ) ;
#27577 = DIRECTION ( 'NONE',  ( 0.000000000000000000, -1.000000000000000000, 1.387778780781445429E-16 ) ) ;
#27578 = ORIENTED_EDGE ( 'NONE', *, *, #24891, .F. ) ;
#27579 = EDGE_CURVE ( 'NONE', #5481, #15436, #24965, .T. ) ;
#27580 = ORIENTED_EDGE ( 'NONE', *, *, #12210, .F. ) ;
#27581 = CARTESIAN_POINT ( 'NONE',  ( 104.4199312700443016, 89.58810137558876363, 100.0000000000000142 ) ) ;
#27582 = LINE ( 'NONE', #14538, #5781 ) ;
#27583 = ORIENTED_EDGE ( 'NONE', *, *, #22723, .T. ) ;
#27584 = ORIENTED_EDGE ( 'NONE', *, *, #20197, .T. ) ;
#27585 = DIRECTION ( 'NONE',  ( -0.8916010070295213863, -0.4528218681379502786, 0.000000000000000000 ) ) ;
#27586 = ADVANCED_FACE ( 'NONE', ( #25170 ), #16559, .F. ) ;
#27587 = VECTOR ( 'NONE', #5963, 1000.000000000000000 ) ;
#27588 = CARTESIAN_POINT ( 'NONE',  ( 109.8784069490710920, 256.7826562374864352, 42.21284981969159844 ) ) ;
#27589 = DIRECTION ( 'NONE',  ( -0.8916010070293383105, -0.4528218681383106015, 0.000000000000000000 ) ) ;
#27590 = VERTEX_POINT ( 'NONE', #6054 ) ;
#27591 = CARTESIAN_POINT ( 'NONE',  ( 157.9999999999996589, 276.1732501651540588, -45.00000000000000000 ) ) ;
#27592 = ORIENTED_EDGE ( 'NONE', *, *, #16469, .F. ) ;
#27593 = VECTOR ( 'NONE', #17704, 1000.000000000000000 ) ;
#27594 = AXIS2_PLACEMENT_3D ( 'NONE', #16825, #12106, #27577 ) ;
#27595 = FACE_OUTER_BOUND ( 'NONE', #76, .T. ) ;
#27596 = CIRCLE ( 'NONE', #15246, 5.000000000000004441 ) ;
#27597 = CARTESIAN_POINT ( 'NONE',  ( 267.4999999999996021, 194.4107529906318064, 288.0938197134494203 ) ) ;
#27598 = CARTESIAN_POINT ( 'NONE',  ( 158.0000000000011084, 98.62199963966197913, 45.00000000000000000 ) ) ;
#27599 = CARTESIAN_POINT ( 'NONE',  ( -43.02437977270766112, 129.7200458115293031, -16.81627168235288394 ) ) ;
#27600 = DIRECTION ( 'NONE',  ( 1.000000000000000000, 0.000000000000000000, -0.000000000000000000 ) ) ;
#27601 = EDGE_CURVE ( 'NONE', #19699, #4657, #8359, .T. ) ;
#27602 = CARTESIAN_POINT ( 'NONE',  ( -112.3221550338875687, 17.24192588826928585, 80.00000000000001421 ) ) ;
#27603 = LINE ( 'NONE', #16570, #23203 ) ;
#27604 = EDGE_LOOP ( 'NONE', ( #16932, #18832, #27464, #10753 ) ) ;
#27605 = EDGE_CURVE ( 'NONE', #21916, #10608, #17851, .T. ) ;
#27606 = CARTESIAN_POINT ( 'NONE',  ( 157.9999999999997726, 246.0787500750700474, 45.00000000000000000 ) ) ;
#27607 = DIRECTION ( 'NONE',  ( 1.000000000000000000, -0.000000000000000000, -0.000000000000000000 ) ) ;
#27608 = FACE_OUTER_BOUND ( 'NONE', #25835, .T. ) ;
#27609 = DIRECTION ( 'NONE',  ( 1.000000000000000000, 0.000000000000000000, 0.000000000000000000 ) ) ;
#27610 = VERTEX_POINT ( 'NONE', #27591 ) ;
#27611 = VECTOR ( 'NONE', #901, 1000.000000000000000 ) ;
#27612 = LINE ( 'NONE', #16855, #1782 ) ;
#27613 = ORIENTED_EDGE ( 'NONE', *, *, #8905, .F. ) ;
#27614 = AXIS2_PLACEMENT_3D ( 'NONE', #4900, #9222, #13690 ) ;
#27615 = CARTESIAN_POINT ( 'NONE',  ( 157.4999999999998579, 90.84443711338730054, -45.00000000000000000 ) ) ;
#27616 = DIRECTION ( 'NONE',  ( 0.8916010070293710621, -0.4528218681382463195, 0.000000000000000000 ) ) ;
#27617 = CARTESIAN_POINT ( 'NONE',  ( 157.9999999999996305, 283.6968751876750616, 45.00000000000000000 ) ) ;
#27618 = ORIENTED_EDGE ( 'NONE', *, *, #24053, .F. ) ;
#27619 = DIRECTION ( 'NONE',  ( 0.000000000000000000, 0.000000000000000000, 1.000000000000000000 ) ) ;
#27620 = LINE ( 'NONE', #21306, #3324 ) ;
#27621 = VERTEX_POINT ( 'NONE', #5490 ) ;
#27622 = EDGE_CURVE ( 'NONE', #7085, #2802, #5635, .T. ) ;
#27623 = AXIS2_PLACEMENT_3D ( 'NONE', #16997, #18732, #23465 ) ;
#27624 = DIRECTION ( 'NONE',  ( -0.000000000000000000, -0.000000000000000000, -1.000000000000000000 ) ) ;
#27625 = FACE_OUTER_BOUND ( 'NONE', #27146, .T. ) ;
#27626 = ORIENTED_EDGE ( 'NONE', *, *, #23067, .F. ) ;
#27627 = VERTEX_POINT ( 'NONE', #14407 ) ;
#27628 = EDGE_CURVE ( 'NONE', #13016, #8625, #23161, .T. ) ;
#27629 = CARTESIAN_POINT ( 'NONE',  ( -68.57415822541635464, -23.01420295945612082, 95.00000000000000000 ) ) ;
#27630 = ORIENTED_EDGE ( 'NONE', *, *, #17635, .F. ) ;
#27631 = EDGE_CURVE ( 'NONE', #27204, #25077, #10512, .T. ) ;
#27632 = VERTEX_POINT ( 'NONE', #16836 ) ;
#27633 = ORIENTED_EDGE ( 'NONE', *, *, #28125, .T. ) ;
#27634 = VECTOR ( 'NONE', #11486, 1000.000000000000000 ) ;
#27635 = DIRECTION ( 'NONE',  ( 1.000000000000000000, 0.000000000000000000, 0.000000000000000000 ) ) ;
#27636 = VECTOR ( 'NONE', #25786, 1000.000000000000227 ) ;
#27637 = LINE ( 'NONE', #16601, #16299 ) ;
#27638 = CYLINDRICAL_SURFACE ( 'NONE', #17897, 5.999999999999977796 ) ;
#27639 = VECTOR ( 'NONE', #4435, 1000.000000000000000 ) ;
#27640 = DIRECTION ( 'NONE',  ( 0.8916010070294498879, -0.4528218681380914434, 0.000000000000000000 ) ) ;
#27641 = CARTESIAN_POINT ( 'NONE',  ( 217.4999999999996305, 83.06687458711267880, 36.86484227207694175 ) ) ;
#27642 = CARTESIAN_POINT ( 'NONE',  ( 282.4999999999996589, 19.41075299063184900, 87.99671038392668265 ) ) ;
#27643 = DIRECTION ( 'NONE',  ( 0.000000000000000000, 0.000000000000000000, 1.000000000000000000 ) ) ;
#27644 = LINE ( 'NONE', #26061, #13874 ) ;
#27645 = LINE ( 'NONE', #19039, #27003 ) ;
#27646 = DIRECTION ( 'NONE',  ( -0.4999999999999919509, 0.8660254037844432595, -1.224646799147353207E-16 ) ) ;
#27647 = ORIENTED_EDGE ( 'NONE', *, *, #3719, .T. ) ;
#27648 = FACE_OUTER_BOUND ( 'NONE', #17039, .T. ) ;
#27649 = DIRECTION ( 'NONE',  ( -0.8916010070293384215, 0.4528218681383106015, 0.000000000000000000 ) ) ;
#27650 = DIRECTION ( 'NONE',  ( 0.000000000000000000, 0.000000000000000000, -1.000000000000000000 ) ) ;
#27651 = FILL_AREA_STYLE ('',( #14464 ) ) ;
#27652 = CARTESIAN_POINT ( 'NONE',  ( 158.0000000000011937, 93.09837461714084839, 45.00000000000000000 ) ) ;
#27653 = ORIENTED_EDGE ( 'NONE', *, *, #17172, .T. ) ;
#27654 = AXIS2_PLACEMENT_3D ( 'NONE', #21457, #1774, #12439 ) ;
#27655 = VECTOR ( 'NONE', #503, 1000.000000000000000 ) ;
#27656 = LINE ( 'NONE', #6257, #27203 ) ;
#27657 = VERTEX_POINT ( 'NONE', #19127 ) ;
#27658 = CARTESIAN_POINT ( 'NONE',  ( -254.3350114625770289, -91.18033988749901653, 0.000000000000000000 ) ) ;
#27659 = ORIENTED_EDGE ( 'NONE', *, *, #12720, .T. ) ;
#27660 = AXIS2_PLACEMENT_3D ( 'NONE', #17764, #26957, #26514 ) ;
#27661 = EDGE_LOOP ( 'NONE', ( #5382, #16127, #5662, #22011, #21036, #13698 ) ) ;
#27662 = ADVANCED_FACE ( 'NONE', ( #5911 ), #21991, .F. ) ;
#27663 = CARTESIAN_POINT ( 'NONE',  ( -175.0000000000000000, -170.0000000000001990, -64.00000000000000000 ) ) ;
#27664 = VERTEX_POINT ( 'NONE', #16701 ) ;
#27665 = ORIENTED_EDGE ( 'NONE', *, *, #20647, .T. ) ;
#27666 = DIRECTION ( 'NONE',  ( -0.000000000000000000, -1.000000000000000000, -0.000000000000000000 ) ) ;
#27667 = LINE ( 'NONE', #8008, #16948 ) ;
#27668 = DIRECTION ( 'NONE',  ( 0.9960550913260672878, 0.000000000000000000, -0.08873699929240064233 ) ) ;
#27669 = CARTESIAN_POINT ( 'NONE',  ( -152.1970234707412146, 122.9096046473621868, -20.33815154695436078 ) ) ;
#27670 = AXIS2_PLACEMENT_3D ( 'NONE', #23554, #6022, #14797 ) ;
#27671 = CARTESIAN_POINT ( 'NONE',  ( -273.6827204801242601, -170.0454132223111969, -86.72642857975071706 ) ) ;
#27672 = CARTESIAN_POINT ( 'NONE',  ( 167.4999999999996589, -5.589247009368157215, 74.99999999999995737 ) ) ;
#27673 = CARTESIAN_POINT ( 'NONE',  ( -274.7077367163463464, -170.0340389212390448, 91.88143064332926713 ) ) ;
#27674 = AXIS2_PLACEMENT_3D ( 'NONE', #13561, #23903, #15434 ) ;
#27675 = PRODUCT_DEFINITION_SHAPE ( 'NONE', 'NONE',  #18451 ) ;
#27676 = EDGE_CURVE ( 'NONE', #27404, #7140, #1784, .T. ) ;
#27677 = CARTESIAN_POINT ( 'NONE',  ( 133.0634450963849531, 249.9396218376480192, -139.3076717160242879 ) ) ;
#27678 = CARTESIAN_POINT ( 'NONE',  ( -216.6938019150388186, 86.34331246501530188, 20.61264131666953503 ) ) ;
#27679 = CIRCLE ( 'NONE', #22667, 5.000000000000000000 ) ;
#27680 = LINE ( 'NONE', #25536, #7864 ) ;
#27681 = LINE ( 'NONE', #25401, #8633 ) ;
#27682 = DIRECTION ( 'NONE',  ( -0.7071067811865489050, 0.000000000000000000, -0.7071067811865462405 ) ) ;
#27683 = ORIENTED_EDGE ( 'NONE', *, *, #11774, .F. ) ;
#27684 = ADVANCED_FACE ( 'NONE', ( #21423 ), #8260, .T. ) ;
#27685 = CARTESIAN_POINT ( 'NONE',  ( 158.0000000000014211, 68.52749954957745615, -45.00000000000000000 ) ) ;
#27686 = CARTESIAN_POINT ( 'NONE',  ( 107.0548155441414195, 209.0846731383313966, -148.9655004847909936 ) ) ;
#27688 = ORIENTED_EDGE ( 'NONE', *, *, #5394, .F. ) ;
#27687 = EDGE_LOOP ( 'NONE', ( #8420, #8001, #8496, #9828 ) ) ;
#27689 = LINE ( 'NONE', #25544, #7905 ) ;
#27690 = ORIENTED_EDGE ( 'NONE', *, *, #21902, .F. ) ;
#27691 = VERTEX_POINT ( 'NONE', #13531 ) ;
#27692 = EDGE_CURVE ( 'NONE', #3711, #8035, #17825, .T. ) ;
#27693 = AXIS2_PLACEMENT_3D ( 'NONE', #4490, #24190, #11415 ) ;
#27694 = ORIENTED_EDGE ( 'NONE', *, *, #26771, .T. ) ;
#27695 = EDGE_CURVE ( 'NONE', #20120, #970, #24866, .T. ) ;
#27696 = EDGE_CURVE ( 'NONE', #25999, #7120, #27012, .T. ) ;
#27697 = VERTEX_POINT ( 'NONE', #9505 ) ;
#27698 = AXIS2_PLACEMENT_3D ( 'NONE', #177, #24449, #8937 ) ;
#27699 = ORIENTED_EDGE ( 'NONE', *, *, #8845, .T. ) ;
#27700 = ORIENTED_EDGE ( 'NONE', *, *, #19042, .F. ) ;
#27701 = CARTESIAN_POINT ( 'NONE',  ( 157.9999999999998010, 241.0630000600560550, -45.00000000000000000 ) ) ;
#27702 = DIRECTION ( 'NONE',  ( -0.000000000000000000, 1.000000000000000000, -1.387778780781445429E-16 ) ) ;
#27703 = CARTESIAN_POINT ( 'NONE',  ( -180.0000000000000284, -40.00000000000004974, 70.00000000000001421 ) ) ;
#27704 = DIRECTION ( 'NONE',  ( -0.000000000000000000, -0.000000000000000000, -1.000000000000000000 ) ) ;
#27705 = CARTESIAN_POINT ( 'NONE',  ( 0.3651377029009472142, -1.250000000000000444, 7.402212548643258394 ) ) ;
#27706 = DIRECTION ( 'NONE',  ( -0.000000000000000000, -0.000000000000000000, -1.000000000000000000 ) ) ;
#27707 = CARTESIAN_POINT ( 'NONE',  ( 157.4999999999998579, 83.32081209086616980, -45.00000000000000000 ) ) ;
#27708 = AXIS2_PLACEMENT_3D ( 'NONE', #25589, #21144, #7936 ) ;
#27709 = CARTESIAN_POINT ( 'NONE',  ( 111.5727331380326319, 201.2585679321024088, -141.0313312019552541 ) ) ;
#27710 = CYLINDRICAL_SURFACE ( 'NONE', #23807, 30.00000000000000000 ) ;
#27711 = CARTESIAN_POINT ( 'NONE',  ( 158.0000000000007958, 130.7164997297464595, 45.00000000000000000 ) ) ;
#27712 = DIRECTION ( 'NONE',  ( 2.775557561562887407E-16, 3.668437989309015850E-32, 1.000000000000000000 ) ) ;
#27713 = VECTOR ( 'NONE', #12315, 1000.000000000000000 ) ;
#27714 = ORIENTED_EDGE ( 'NONE', *, *, #1241, .T. ) ;
#27715 = CARTESIAN_POINT ( 'NONE',  ( -191.5190414516356441, 102.2994403167507329, 32.46908855772340985 ) ) ;
#27716 = EDGE_CURVE ( 'NONE', #15041, #11767, #2883, .T. ) ;
#27717 = EDGE_CURVE ( 'NONE', #2802, #3882, #9067, .T. ) ;
#27718 = FACE_OUTER_BOUND ( 'NONE', #9348, .T. ) ;
#27719 = EDGE_LOOP ( 'NONE', ( #22422, #7892, #12706, #8172 ) ) ;
#27720 = APPLICATION_PROTOCOL_DEFINITION ( 'draft international standard', 'automotive_design', 1998, #13339 ) ;
#27721 = ORIENTED_EDGE ( 'NONE', *, *, #11937, .T. ) ;
#27722 = EDGE_LOOP ( 'NONE', ( #10723, #28310, #3506, #12541 ) ) ;
#27723 = LINE ( 'NONE', #8064, #25759 ) ;
#27724 = CARTESIAN_POINT ( 'NONE',  ( -260.0000000000001137, -165.0000000000000853, 60.00000000000002132 ) ) ;
#27725 = EDGE_CURVE ( 'NONE', #27697, #7120, #7346, .T. ) ;
#27726 = ORIENTED_EDGE ( 'NONE', *, *, #18724, .T. ) ;
#27727 = VECTOR ( 'NONE', #18336, 1000.000000000000000 ) ;
#27728 = VECTOR ( 'NONE', #6306, 1000.000000000000000 ) ;
#27729 = EDGE_LOOP ( 'NONE', ( #10293, #19541, #9847, #18063 ) ) ;
#27730 = FACE_OUTER_BOUND ( 'NONE', #23858, .T. ) ;
#27731 = ADVANCED_FACE ( 'NONE', ( #18262 ), #22282, .F. ) ;
#27732 = MANIFOLD_SOLID_BREP ( 'Fillet9', #20051 ) ;
#27733 = PLANE ( 'NONE',  #1499 ) ;
#27734 = CYLINDRICAL_SURFACE ( 'NONE', #6373, 5.000000000000004441 ) ;
#27735 = ORIENTED_EDGE ( 'NONE', *, *, #6908, .T. ) ;
#27736 = CARTESIAN_POINT ( 'NONE',  ( -231.9378824387731015, 93.53122965655664700, 14.99999999999999289 ) ) ;
#27737 = EDGE_LOOP ( 'NONE', ( #21307, #25564, #5801, #23898 ) ) ;
#27738 = AXIS2_PLACEMENT_3D ( 'NONE', #17450, #5969, #15318 ) ;
#27739 = CARTESIAN_POINT ( 'NONE',  ( -213.1827219047386848, -216.7767438708612531, -110.0000000000000284 ) ) ;
#27740 = LINE ( 'NONE', #13079, #21365 ) ;
#27741 = DIRECTION ( 'NONE',  ( -0.2500000000000127121, 0.000000000000000000, -0.9682458365518510357 ) ) ;
#27742 = CARTESIAN_POINT ( 'NONE',  ( 158.0000000000004263, 168.3346248423521274, 45.00000000000000000 ) ) ;
#27743 = PLANE ( 'NONE',  #9130 ) ;
#27744 = LINE ( 'NONE', #10523, #2795 ) ;
#27745 = CARTESIAN_POINT ( 'NONE',  ( -201.6488700512677212, 93.99433454770324659, -30.47120949752622820 ) ) ;
#27746 = ORIENTED_EDGE ( 'NONE', *, *, #13524, .F. ) ;
#27747 = CARTESIAN_POINT ( 'NONE',  ( 158.0000000000002274, 183.8897498949014278, -45.00000000000000000 ) ) ;
#27748 = CIRCLE ( 'NONE', #2992, 44.99999999999998579 ) ;
#27749 = DIRECTION ( 'NONE',  ( 1.000000000000000000, 0.000000000000000000, -0.000000000000000000 ) ) ;
#27750 = CARTESIAN_POINT ( 'NONE',  ( 158.0000000000007958, 130.7164997297464595, 45.00000000000000000 ) ) ;
#27751 = DIRECTION ( 'NONE',  ( 0.000000000000000000, 9.251858538542967883E-17, -1.000000000000000000 ) ) ;
#27752 = VERTEX_POINT ( 'NONE', #15499 ) ;
#27753 = CARTESIAN_POINT ( 'NONE',  ( 157.4999999999997442, 251.3484375938375024, 45.00000000000000000 ) ) ;
#27754 = ORIENTED_EDGE ( 'NONE', *, *, #4702, .F. ) ;
#27755 = EDGE_CURVE ( 'NONE', #5560, #15143, #13677, .T. ) ;
#27756 = PLANE ( 'NONE',  #1078 ) ;
#27757 = DIRECTION ( 'NONE',  ( 4.625929269271489858E-16, -2.100614451407711032E-31, 1.000000000000000000 ) ) ;
#27758 = CARTESIAN_POINT ( 'NONE',  ( -209.0203365101457109, 89.44154586134021656, 24.30531738582797274 ) ) ;
#27759 = ORIENTED_EDGE ( 'NONE', *, *, #7742, .F. ) ;
#27760 = DIRECTION ( 'NONE',  ( -3.053113317719176147E-15, -4.035281788239917819E-31, -1.000000000000000000 ) ) ;
#27761 = CARTESIAN_POINT ( 'NONE',  ( 119.1329331941752230, 232.1752285801739220, 45.00000000000000000 ) ) ;
#27762 = AXIS2_PLACEMENT_3D ( 'NONE', #15577, #21890, #13282 ) ;
#27763 = ORIENTED_EDGE ( 'NONE', *, *, #3460, .F. ) ;
#27764 = CARTESIAN_POINT ( 'NONE',  ( -157.8108137764193373, 120.7058031521935391, 21.99230116549754399 ) ) ;
#27765 = DIRECTION ( 'NONE',  ( -0.8916010070295004031, 0.4528218681379916344, 0.000000000000000000 ) ) ;
#27766 = ORIENTED_EDGE ( 'NONE', *, *, #12133, .F. ) ;
#27767 = ORIENTED_EDGE ( 'NONE', *, *, #24014, .T. ) ;
#27768 = CARTESIAN_POINT ( 'NONE',  ( 232.4999999999996305, 133.0668745871126930, 42.88984227207694744 ) ) ;
#27769 = ORIENTED_EDGE ( 'NONE', *, *, #28335, .T. ) ;
#27770 = ADVANCED_FACE ( 'NONE', ( #17638 ), #2541, .F. ) ;
#27771 = EDGE_CURVE ( 'NONE', #25890, #27860, #26110, .T. ) ;
#27772 = VECTOR ( 'NONE', #12481, 1000.000000000000000 ) ;
#27773 = ORIENTED_EDGE ( 'NONE', *, *, #26700, .F. ) ;
#27774 = ORIENTED_EDGE ( 'NONE', *, *, #4257, .T. ) ;
#27775 = AXIS2_PLACEMENT_3D ( 'NONE', #21465, #10558, #6100 ) ;
#27776 = AXIS2_PLACEMENT_3D ( 'NONE', #27377, #7719, #16485 ) ;
#27777 = CARTESIAN_POINT ( 'NONE',  ( 65.00000000000000000, -170.0000000000000568, 76.00000000000000000 ) ) ;
#27778 = LINE ( 'NONE', #10411, #710 ) ;
#27779 = LINE ( 'NONE', #7976, #1827 ) ;
#27780 = VECTOR ( 'NONE', #1262, 999.9999999999998863 ) ;
#27781 = EDGE_CURVE ( 'NONE', #20027, #14958, #13480, .T. ) ;
#27782 = DIRECTION ( 'NONE',  ( 0.000000000000000000, -1.000000000000000000, -1.214306433183764966E-16 ) ) ;
#27783 = CARTESIAN_POINT ( 'NONE',  ( -175.0000000000000000, -173.6051637141655704, -69.99999999999998579 ) ) ;
#27784 = CARTESIAN_POINT ( 'NONE',  ( -231.0952835391973963, 75.72709865443405874, -15.86948571459950053 ) ) ;
#27785 = EDGE_CURVE ( 'NONE', #18799, #3986, #23947, .T. ) ;
#27786 = CYLINDRICAL_SURFACE ( 'NONE', #305, 5.000000000000000888 ) ;
#27787 = DIRECTION ( 'NONE',  ( -0.8916010070293584056, -0.4528218681382712996, 0.000000000000000000 ) ) ;
#27788 = DIRECTION ( 'NONE',  ( 1.000000000000000000, 0.000000000000000000, 0.000000000000000000 ) ) ;
#27789 = DIRECTION ( 'NONE',  ( 0.8660254037844432595, 0.4999999999999919509, -0.000000000000000000 ) ) ;
#27790 = ORIENTED_EDGE ( 'NONE', *, *, #11547, .F. ) ;
#27791 = DIRECTION ( 'NONE',  ( -0.8379557447115515423, 0.5457381880580733924, 0.000000000000000000 ) ) ;
#27792 = PLANE ( 'NONE',  #4577 ) ;
#27793 = CARTESIAN_POINT ( 'NONE',  ( 158.0000000000013358, 80.55899957960563995, 45.00000000000000000 ) ) ;
#27794 = EDGE_CURVE ( 'NONE', #8019, #9011, #13067, .T. ) ;
#27795 = CARTESIAN_POINT ( 'NONE',  ( 157.4999999999998579, 151.0334372935563465, -45.00000000000000000 ) ) ;
#27796 = ORIENTED_EDGE ( 'NONE', *, *, #13622, .T. ) ;
#27797 = AXIS2_PLACEMENT_3D ( 'NONE', #26643, #2224, #373 ) ;
#27798 = CARTESIAN_POINT ( 'NONE',  ( -236.8177751472017007, 82.33896643611701904, 15.00000000000000000 ) ) ;
#27799 = ORIENTED_EDGE ( 'NONE', *, *, #9683, .T. ) ;
#27800 = DIRECTION ( 'NONE',  ( 0.9659258262890662028, -0.2588190451025286221, 0.000000000000000000 ) ) ;
#27801 = ORIENTED_EDGE ( 'NONE', *, *, #26805, .T. ) ;
#27802 = TOROIDAL_SURFACE ( 'NONE', #15443, 7.509856658345970715, 10.53396790234564762 ) ;
#27803 = ORIENTED_EDGE ( 'NONE', *, *, #15149, .F. ) ;
#27804 = LINE ( 'NONE', #5840, #11777 ) ;
#27805 = VERTEX_POINT ( 'NONE', #6859 ) ;
#27806 = ORIENTED_EDGE ( 'NONE', *, *, #17610, .F. ) ;
#27807 = CARTESIAN_POINT ( 'NONE',  ( 158.0000000000010516, 103.6377496546760568, 45.00000000000000000 ) ) ;
#27808 = CARTESIAN_POINT ( 'NONE',  ( -47.91415621944423719, 130.8825976540551608, -16.39223340224337733 ) ) ;
#27809 = CARTESIAN_POINT ( 'NONE',  ( -210.0000000000000568, -220.0000000000000853, 90.87829376371914236 ) ) ;
#27810 = CARTESIAN_POINT ( 'NONE',  ( -127.4043536527376688, 130.3575739508328013, -16.56241948173741463 ) ) ;
#27811 = AXIS2_PLACEMENT_3D ( 'NONE', #20333, #18329, #20189 ) ;
#27812 = DIRECTION ( 'NONE',  ( -0.000000000000000000, -0.000000000000000000, -1.000000000000000000 ) ) ;
#27813 = LINE ( 'NONE', #20658, #11413 ) ;
#27814 = CARTESIAN_POINT ( 'NONE',  ( 32.36067977499786252, -40.00000000000003553, 100.0000000000000142 ) ) ;
#27815 = CARTESIAN_POINT ( 'NONE',  ( -230.8931271727480805, 92.61283034429897043, -15.05361674725927301 ) ) ;
#27816 = CARTESIAN_POINT ( 'NONE',  ( 131.8275543060484267, 249.8322405497061993, -139.9035143180224736 ) ) ;
#27817 = CARTESIAN_POINT ( 'NONE',  ( -226.2800442625073174, 87.57925215467369640, 16.13539826775552299 ) ) ;
#27818 = CARTESIAN_POINT ( 'NONE',  ( 217.4999999999996305, 494.4107529906318632, -100.0000000000000142 ) ) ;
#27819 = FACE_OUTER_BOUND ( 'NONE', #26573, .T. ) ;
#27820 = CARTESIAN_POINT ( 'NONE',  ( 128.0812361363527998, 241.9574749595457774, 45.00000000000000000 ) ) ;
#27821 = EDGE_CURVE ( 'NONE', #9740, #17744, #4281, .T. ) ;
#27822 = ORIENTED_EDGE ( 'NONE', *, *, #14581, .F. ) ;
#27823 = EDGE_CURVE ( 'NONE', #13440, #1333, #26577, .T. ) ;
#27824 = LINE ( 'NONE', #27685, #22909 ) ;
#27825 = EDGE_CURVE ( 'NONE', #1063, #3920, #16889, .T. ) ;
#27826 = DIRECTION ( 'NONE',  ( 0.000000000000000000, 0.000000000000000000, 1.000000000000000000 ) ) ;
#27828 = ORIENTED_EDGE ( 'NONE', *, *, #6135, .F. ) ;
#27827 = ORIENTED_EDGE ( 'NONE', *, *, #24606, .F. ) ;
#27829 = CARTESIAN_POINT ( 'NONE',  ( 104.2862437451156126, 245.6633304404597595, -27.19020029359707991 ) ) ;
#27830 = EDGE_LOOP ( 'NONE', ( #13134, #13774, #3010 ) ) ;
#27831 = ORIENTED_EDGE ( 'NONE', *, *, #5826, .T. ) ;
#27832 = VECTOR ( 'NONE', #9209, 1000.000000000000000 ) ;
#27833 = EDGE_LOOP ( 'NONE', ( #18038, #16179, #11830, #7441 ) ) ;
#27834 = CIRCLE ( 'NONE', #19131, 6.025000000000002132 ) ;
#27835 = ORIENTED_EDGE ( 'NONE', *, *, #2197, .F. ) ;
#27836 = ORIENTED_EDGE ( 'NONE', *, *, #25848, .T. ) ;
#27837 = ORIENTED_EDGE ( 'NONE', *, *, #8053, .T. ) ;
#27838 = DIRECTION ( 'NONE',  ( 1.000000000000000000, 0.000000000000000000, 0.000000000000000000 ) ) ;
#27839 = LINE ( 'NONE', #27984, #13765 ) ;
#27840 = DIRECTION ( 'NONE',  ( 1.000000000000000000, 0.000000000000000000, -0.000000000000000000 ) ) ;
#27841 = DIRECTION ( 'NONE',  ( 0.000000000000000000, 0.000000000000000000, -1.000000000000000000 ) ) ;
#27842 = CARTESIAN_POINT ( 'NONE',  ( -305.0000000000001137, -152.0000000000000284, 60.00000000000001421 ) ) ;
#27843 = EDGE_CURVE ( 'NONE', #8245, #18572, #7298, .T. ) ;
#27844 = CARTESIAN_POINT ( 'NONE',  ( -210.0000000000000568, -280.0000000000000000, 110.0000000000000284 ) ) ;
#27845 = AXIS2_PLACEMENT_3D ( 'NONE', #8036, #7623, #10336 ) ;
#27846 = DIRECTION ( 'NONE',  ( 1.000000000000000000, 0.000000000000000000, 0.000000000000000000 ) ) ;
#27847 = EDGE_CURVE ( 'NONE', #23150, #268, #16352, .T. ) ;
#27848 = EDGE_CURVE ( 'NONE', #7637, #17545, #7729, .T. ) ;
#27849 = DIRECTION ( 'NONE',  ( 0.9784193629480785193, -0.2066290158914672881, 0.000000000000000000 ) ) ;
#27850 = EDGE_CURVE ( 'NONE', #27055, #7931, #20553, .T. ) ;
#27851 = FACE_OUTER_BOUND ( 'NONE', #11396, .T. ) ;
#27852 = CARTESIAN_POINT ( 'NONE',  ( -146.6428522700808230, 69.54464929955099706, 83.00000000000001421 ) ) ;
#27853 = DIRECTION ( 'NONE',  ( 0.000000000000000000, -1.000000000000000000, 0.000000000000000000 ) ) ;
#27854 = VERTEX_POINT ( 'NONE', #13632 ) ;
#27855 = DIRECTION ( 'NONE',  ( -0.000000000000000000, -0.000000000000000000, -1.000000000000000000 ) ) ;
#27856 = CARTESIAN_POINT ( 'NONE',  ( 109.9999999999999005, 3.816391647148972452E-14, 100.0000000000000142 ) ) ;
#27857 = ORIENTED_EDGE ( 'NONE', *, *, #18909, .F. ) ;
#27858 = SHAPE_DEFINITION_REPRESENTATION ( #21977, #13220 ) ;
#27859 = ORIENTED_EDGE ( 'NONE', *, *, #23217, .F. ) ;
#27860 = VERTEX_POINT ( 'NONE', #9311 ) ;
#27861 = AXIS2_PLACEMENT_3D ( 'NONE', #4575, #10772, #21538 ) ;
#27862 = CARTESIAN_POINT ( 'NONE',  ( 157.4999999999998579, 70.78143705333094715, -45.00000000000000000 ) ) ;
#27863 = LINE ( 'NONE', #21557, #22316 ) ;
#27864 = ORIENTED_EDGE ( 'NONE', *, *, #24633, .T. ) ;
#27865 = ORIENTED_EDGE ( 'NONE', *, *, #8729, .T. ) ;
#27866 = CARTESIAN_POINT ( 'NONE',  ( 217.4999999999996305, 83.06687458711267880, -42.86484227207692754 ) ) ;
#27867 = DIRECTION ( 'NONE',  ( 1.000000000000000000, 0.000000000000000000, 0.000000000000000000 ) ) ;
#27868 = CARTESIAN_POINT ( 'NONE',  ( -186.8771810018902499, 105.5597884250916678, -31.69226466690710353 ) ) ;
#27869 = ORIENTED_EDGE ( 'NONE', *, *, #22198, .T. ) ;
#27870 = DIRECTION ( 'NONE',  ( 0.4999999999999985012, -0.8660254037844394848, 0.000000000000000000 ) ) ;
#27871 = VERTEX_POINT ( 'NONE', #13921 ) ;
#27872 = CARTESIAN_POINT ( 'NONE',  ( 147.1752285801741493, 235.8670668058244644, 45.00000000000000000 ) ) ;
#27873 = ADVANCED_FACE ( 'NONE', ( #3250 ), #18074, .F. ) ;
#27874 = ADVANCED_FACE ( 'NONE', ( #11902 ), #11765, .F. ) ;
#27875 = CIRCLE ( 'NONE', #13706, 9.999999999999985789 ) ;
#27876 = DIRECTION ( 'NONE',  ( 0.000000000000000000, 0.000000000000000000, -1.000000000000000000 ) ) ;
#27877 = CARTESIAN_POINT ( 'NONE',  ( 158.0000000000007390, 133.7322497447605656, 45.00000000000000000 ) ) ;
#27878 = CARTESIAN_POINT ( 'NONE',  ( -42.53273978471831640, 130.9733465240572627, -14.93735646117640492 ) ) ;
#27879 = EDGE_CURVE ( 'NONE', #23150, #6357, #21475, .T. ) ;
#27880 = DIRECTION ( 'NONE',  ( 1.850371707708594316E-16, -1.000000000000000000, 0.000000000000000000 ) ) ;
#27881 = DIRECTION ( 'NONE',  ( 0.000000000000000000, -1.000000000000000000, 0.000000000000000000 ) ) ;
#27882 = VECTOR ( 'NONE', #3661, 1000.000000000000000 ) ;
#27883 = ORIENTED_EDGE ( 'NONE', *, *, #13572, .F. ) ;
#27884 = DIRECTION ( 'NONE',  ( 0.000000000000000000, 0.000000000000000000, -1.000000000000000000 ) ) ;
#27885 = EDGE_CURVE ( 'NONE', #5248, #18456, #27875, .T. ) ;
#27886 = CIRCLE ( 'NONE', #22864, 10.00000000000000888 ) ;
#27887 = DIRECTION ( 'NONE',  ( -0.000000000000000000, 0.000000000000000000, -1.000000000000000000 ) ) ;
#27888 = CARTESIAN_POINT ( 'NONE',  ( 158.0000000000001705, 190.9054999099155054, 45.00000000000000000 ) ) ;
#27889 = CARTESIAN_POINT ( 'NONE',  ( -180.0000000000000284, -50.00000000000004263, 98.28427124746191623 ) ) ;
#27890 = ORIENTED_EDGE ( 'NONE', *, *, #13350, .F. ) ;
#27891 = LINE ( 'NONE', #12277, #12371 ) ;
#27892 = LINE ( 'NONE', #8095, #4737 ) ;
#27893 = DIRECTION ( 'NONE',  ( 0.000000000000000000, -1.000000000000000000, 0.000000000000000000 ) ) ;
#27894 = CARTESIAN_POINT ( 'NONE',  ( -210.0000000000000568, -157.0000000000000284, 110.0000000000000284 ) ) ;
#27895 = ORIENTED_EDGE ( 'NONE', *, *, #26928, .F. ) ;
#27896 = PLANE ( 'NONE',  #27623 ) ;
#27897 = VERTEX_POINT ( 'NONE', #20504 ) ;
#27898 = CARTESIAN_POINT ( 'NONE',  ( 157.9999999999996305, 281.6968751876750616, -45.00000000000000000 ) ) ;
#27899 = CARTESIAN_POINT ( 'NONE',  ( 158.0000000000014495, 68.01962454207041731, -45.00000000000000000 ) ) ;
#27900 = ORIENTED_EDGE ( 'NONE', *, *, #24812, .T. ) ;
#27901 = VERTEX_POINT ( 'NONE', #2974 ) ;
#27902 = CARTESIAN_POINT ( 'NONE',  ( -241.9743096803475453, -91.18033988749901653, 0.000000000000000000 ) ) ;
#27903 = EDGE_LOOP ( 'NONE', ( #17480, #1781, #20019, #24252 ) ) ;
#27904 = VECTOR ( 'NONE', #19175, 1000.000000000000000 ) ;
#27905 = AXIS2_PLACEMENT_3D ( 'NONE', #18578, #27191, #4924 ) ;
#27906 = ORIENTED_EDGE ( 'NONE', *, *, #12211, .T. ) ;
#27907 = ORIENTED_EDGE ( 'NONE', *, *, #18143, .F. ) ;
#27908 = DIRECTION ( 'NONE',  ( -0.000000000000000000, -1.000000000000000000, -0.000000000000000000 ) ) ;
#27909 = VECTOR ( 'NONE', #14266, 1000.000000000000000 ) ;
#27910 = EDGE_CURVE ( 'NONE', #5522, #14116, #5411, .T. ) ;
#27911 = PLANE ( 'NONE',  #19507 ) ;
#27912 = LINE ( 'NONE', #4218, #22197 ) ;
#27913 = DIRECTION ( 'NONE',  ( 0.000000000000000000, 0.000000000000000000, -1.000000000000000000 ) ) ;
#27914 = CARTESIAN_POINT ( 'NONE',  ( 119.9999999999999005, 203.2294901687515960, -100.0000000000000142 ) ) ;
#27915 = FACE_OUTER_BOUND ( 'NONE', #447, .T. ) ;
#27916 = CARTESIAN_POINT ( 'NONE',  ( -216.3288264717409106, 60.34946693787968286, -12.99564918865353569 ) ) ;
#27917 = ORIENTED_EDGE ( 'NONE', *, *, #109, .F. ) ;
#27918 = MANIFOLD_SOLID_BREP ( 'Chamfer1', #26016 ) ;
#27919 = VECTOR ( 'NONE', #18449, 1000.000000000000227 ) ;
#27920 = CARTESIAN_POINT ( 'NONE',  ( 136.0000000000000853, 196.9999999999997442, 45.00000000000000000 ) ) ;
#27921 = CARTESIAN_POINT ( 'NONE',  ( 157.4999999999998579, 98.36806213590843129, 45.00000000000000000 ) ) ;
#27922 = DIRECTION ( 'NONE',  ( -0.000000000000000000, 1.000000000000000000, -1.387778780781445429E-16 ) ) ;
#27923 = CARTESIAN_POINT ( 'NONE',  ( 112.5004877479093892, 221.0403377251794836, -96.61493133138624501 ) ) ;
#27924 = ORIENTED_EDGE ( 'NONE', *, *, #5449, .F. ) ;
#27925 = DIRECTION ( 'NONE',  ( 0.000000000000000000, -1.000000000000000000, 0.000000000000000000 ) ) ;
#27926 = AXIS2_PLACEMENT_3D ( 'NONE', #8162, #21374, #1690 ) ;
#27927 = EDGE_CURVE ( 'NONE', #3903, #4479, #12040, .T. ) ;
#27928 = LINE ( 'NONE', #6113, #6999 ) ;
#27929 = SPHERICAL_SURFACE ( 'NONE', #19717, 5.000000000000000000 ) ;
#27930 = DIRECTION ( 'NONE',  ( 0.000000000000000000, -1.000000000000000000, 0.000000000000000000 ) ) ;
#27931 = CARTESIAN_POINT ( 'NONE',  ( 157.9999999999996589, 279.1890001801680796, -45.00000000000000000 ) ) ;
#27932 = ORIENTED_EDGE ( 'NONE', *, *, #508, .F. ) ;
#27933 = CIRCLE ( 'NONE', #7334, 9.999999999999996447 ) ;
#27934 = DIRECTION ( 'NONE',  ( -0.8660254037844394848, -0.4999999999999985012, 0.000000000000000000 ) ) ;
#27935 = ORIENTED_EDGE ( 'NONE', *, *, #13063, .F. ) ;
#27936 = FACE_OUTER_BOUND ( 'NONE', #28261, .T. ) ;
#27937 = ORIENTED_EDGE ( 'NONE', *, *, #23856, .T. ) ;
#27938 = EDGE_CURVE ( 'NONE', #23833, #13994, #9460, .T. ) ;
#27939 = ORIENTED_EDGE ( 'NONE', *, *, #26142, .F. ) ;
#27940 = DIRECTION ( 'NONE',  ( 1.000000000000000000, 0.000000000000000000, -0.000000000000000000 ) ) ;
#27941 = VECTOR ( 'NONE', #15389, 1000.000000000000000 ) ;
#27942 = AXIS2_PLACEMENT_3D ( 'NONE', #16978, #1183, #23586 ) ;
#27943 = ORIENTED_EDGE ( 'NONE', *, *, #16810, .F. ) ;
#27944 = ORIENTED_EDGE ( 'NONE', *, *, #67, .T. ) ;
#27945 = CARTESIAN_POINT ( 'NONE',  ( 113.9142275403300459, 212.0873699598490134, 97.94883453769585913 ) ) ;
#27946 = DIRECTION ( 'NONE',  ( -0.8916010070293409751, -0.4528218681383056610, 0.000000000000000000 ) ) ;
#27947 = VECTOR ( 'NONE', #28072, 1000.000000000000000 ) ;
#27948 = EDGE_CURVE ( 'NONE', #6335, #620, #24961, .T. ) ;
#27949 = FACE_OUTER_BOUND ( 'NONE', #4311, .T. ) ;
#27950 = VECTOR ( 'NONE', #14619, 1000.000000000000000 ) ;
#27951 = CARTESIAN_POINT ( 'NONE',  ( -274.7557459110829541, -165.0000000000001137, -86.12025961983451339 ) ) ;
#27952 = CARTESIAN_POINT ( 'NONE',  ( 158.0000000000016200, 50.97237449702815582, 45.00000000000000000 ) ) ;
#27953 = CARTESIAN_POINT ( 'NONE',  ( 28.53653844984206955, -43.59399515434488137, 99.78583825828528120 ) ) ;
#27954 = CARTESIAN_POINT ( 'NONE',  ( -216.2184996979340497, 87.78057762432685251, -20.45253552124680851 ) ) ;
#27955 = LINE ( 'NONE', #12341, #8544 ) ;
#27956 = CARTESIAN_POINT ( 'NONE',  ( -233.2943309833541718, 92.06151970357194614, 15.00000000000000000 ) ) ;
#27957 = DIRECTION ( 'NONE',  ( -0.000000000000000000, -0.000000000000000000, -1.000000000000000000 ) ) ;
#27958 = DIRECTION ( 'NONE',  ( 1.000000000000000000, 0.000000000000000000, 0.000000000000000000 ) ) ;
#27959 = DIRECTION ( 'NONE',  ( 1.000000000000000000, 0.000000000000000000, 0.000000000000000000 ) ) ;
#27960 = EDGE_LOOP ( 'NONE', ( #370, #6289 ) ) ;
#27961 = EDGE_CURVE ( 'NONE', #21738, #22565, #6116, .T. ) ;
#27962 = EDGE_CURVE ( 'NONE', #16662, #4224, #17871, .T. ) ;
#27963 = VECTOR ( 'NONE', #27812, 1000.000000000000000 ) ;
#27964 = DIRECTION ( 'NONE',  ( 0.000000000000000000, 1.000000000000000000, 0.000000000000000000 ) ) ;
#27965 = CARTESIAN_POINT ( 'NONE',  ( -279.3160071107327553, -91.18033988749907337, 0.000000000000000000 ) ) ;
#27966 = CARTESIAN_POINT ( 'NONE',  ( 108.0238497313615227, 206.8729107250730408, -150.6165463336312769 ) ) ;
#27968 = ORIENTED_EDGE ( 'NONE', *, *, #22133, .T. ) ;
#27967 = ORIENTED_EDGE ( 'NONE', *, *, #14168, .T. ) ;
#27969 = CIRCLE ( 'NONE', #22949, 33.76444293738739333 ) ;
#27970 = MANIFOLD_SOLID_BREP ( '\X2\00d8\X0\12.0mm Dowel Hole3[2]', #3996 ) ;
#27971 = CARTESIAN_POINT ( 'NONE',  ( 94.98941689213211248, 231.7050943134732108, -19.00901305069148961 ) ) ;
#27972 = ORIENTED_EDGE ( 'NONE', *, *, #23541, .T. ) ;
#27973 = ORIENTED_EDGE ( 'NONE', *, *, #25915, .F. ) ;
#27974 = ORIENTED_EDGE ( 'NONE', *, *, #18190, .F. ) ;
#27975 = EDGE_CURVE ( 'NONE', #18824, #13911, #27512, .T. ) ;
#27976 = ORIENTED_EDGE ( 'NONE', *, *, #11863, .T. ) ;
#27977 = EDGE_LOOP ( 'NONE', ( #24013, #17453, #14903, #1199 ) ) ;
#27978 = ORIENTED_EDGE ( 'NONE', *, *, #4780, .F. ) ;
#27979 = ORIENTED_EDGE ( 'NONE', *, *, #1295, .F. ) ;
#27980 = EDGE_CURVE ( 'NONE', #24009, #8550, #20920, .T. ) ;
#27981 = LINE ( 'NONE', #21392, #25559 ) ;
#27982 = EDGE_CURVE ( 'NONE', #12064, #19409, #8131, .T. ) ;
#27983 = VECTOR ( 'NONE', #20052, 1000.000000000000000 ) ;
#27984 = CARTESIAN_POINT ( 'NONE',  ( 157.4999999999996589, 276.4271876689075498, -45.00000000000000000 ) ) ;
#27985 = ADVANCED_FACE ( 'NONE', ( #25229 ), #1239, .T. ) ;
#27986 = CARTESIAN_POINT ( 'NONE',  ( 158.0000000000000853, 196.4291249324366504, 45.00000000000000000 ) ) ;
#27987 = VECTOR ( 'NONE', #3766, 1000.000000000000000 ) ;
#27988 = LINE ( 'NONE', #8327, #14258 ) ;
#27989 = CARTESIAN_POINT ( 'NONE',  ( 134.9999999999998579, 220.0000000000000284, -99.00000000000001421 ) ) ;
#27990 = CARTESIAN_POINT ( 'NONE',  ( -107.3221550338875687, 22.24192588826928585, 83.00000000000001421 ) ) ;
#27991 = CYLINDRICAL_SURFACE ( 'NONE', #4252, 16.46313063346208239 ) ;
#27992 = CARTESIAN_POINT ( 'NONE',  ( -38.26150398323100887, 130.0131485130493729, 16.67769045341279011 ) ) ;
#27993 = LINE ( 'NONE', #20976, #11437 ) ;
#27994 = EDGE_CURVE ( 'NONE', #1940, #6895, #16003, .T. ) ;
#27995 = FACE_OUTER_BOUND ( 'NONE', #3082, .T. ) ;
#27996 = DIRECTION ( 'NONE',  ( 1.000000000000000000, 0.000000000000000000, 0.000000000000000000 ) ) ;
#27997 = VERTEX_POINT ( 'NONE', #7846 ) ;
#27998 = FACE_OUTER_BOUND ( 'NONE', #10119, .T. ) ;
#27999 = AXIS2_PLACEMENT_3D ( 'NONE', #25592, #7802, #7940 ) ;
#28000 = DIRECTION ( 'NONE',  ( -0.000000000000000000, -0.000000000000000000, -1.000000000000000000 ) ) ;
#28001 = ORIENTED_EDGE ( 'NONE', *, *, #14999, .F. ) ;
#28002 = CONTEXT_DEPENDENT_SHAPE_REPRESENTATION ( #28157, #19448 ) ;
#28003 = VERTEX_POINT ( 'NONE', #8275 ) ;
#28004 = ORIENTED_EDGE ( 'NONE', *, *, #10419, .F. ) ;
#28005 = AXIS2_PLACEMENT_3D ( 'NONE', #6346, #10384, #19140 ) ;
#28006 = CARTESIAN_POINT ( 'NONE',  ( 82.91040908012763566, 80.00000000660637056, 100.0000000000000142 ) ) ;
#28007 = LINE ( 'NONE', #12677, #4880 ) ;
#28008 = ORIENTED_EDGE ( 'NONE', *, *, #26454, .F. ) ;
#28009 = VERTEX_POINT ( 'NONE', #25372 ) ;
#28010 = ADVANCED_FACE ( 'NONE', ( #10008 ), #7990, .T. ) ;
#28011 = CARTESIAN_POINT ( 'NONE',  ( 105.2480867101029531, 123.6573351780301095, -85.93750000029402258 ) ) ;
#28012 = EDGE_CURVE ( 'NONE', #8519, #23293, #6338, .T. ) ;
#28013 = MANIFOLD_SOLID_BREP ( '\X2\00d8\X0\12.0mm Dowel Hole3[1]', #1702 ) ;
#28014 = DIRECTION ( 'NONE',  ( -1.000000000000000000, 0.000000000000000000, -0.000000000000000000 ) ) ;
#28015 = DIRECTION ( 'NONE',  ( -0.000000000000000000, -0.000000000000000000, -1.000000000000000000 ) ) ;
#28016 = VERTEX_POINT ( 'NONE', #4095 ) ;
#28017 = CARTESIAN_POINT ( 'NONE',  ( 113.4920585194047078, 104.4775165427241319, 100.0000000000000142 ) ) ;
#28018 = ORIENTED_EDGE ( 'NONE', *, *, #3997, .T. ) ;
#28019 = DIRECTION ( 'NONE',  ( 0.000000000000000000, 0.000000000000000000, 1.000000000000000000 ) ) ;
#28020 = PLANE ( 'NONE',  #26810 ) ;
#28021 = CARTESIAN_POINT ( 'NONE',  ( -210.0000000000000568, -220.0000000000000853, -110.0000000000000284 ) ) ;
#28022 = PLANE ( 'NONE',  #17934 ) ;
#28023 = AXIS2_PLACEMENT_3D ( 'NONE', #2454, #4756, #4607 ) ;
#28024 = ORIENTED_EDGE ( 'NONE', *, *, #15800, .F. ) ;
#28025 = CYLINDRICAL_SURFACE ( 'NONE', #15993, 22.49999999999999289 ) ;
#28026 = ADVANCED_FACE ( 'NONE', ( #26484 ), #25789, .F. ) ;
#28027 = LINE ( 'NONE', #17547, #17011 ) ;
#28028 = DIRECTION ( 'NONE',  ( 0.7071067811865335839, -0.7071067811865613395, 0.000000000000000000 ) ) ;
#28029 = CARTESIAN_POINT ( 'NONE',  ( -180.0000000000000284, -70.00000000000004263, 70.00000000000000000 ) ) ;
#28030 = ORIENTED_EDGE ( 'NONE', *, *, #16693, .T. ) ;
#28031 = DIRECTION ( 'NONE',  ( 0.8916010070299571488, -0.4528218681370922982, 0.000000000000000000 ) ) ;
#28032 = CARTESIAN_POINT ( 'NONE',  ( -254.4816742664885965, 103.7585653882801182, 5.000000000000002665 ) ) ;
#28033 = DIRECTION ( 'NONE',  ( -0.000000000000000000, 0.000000000000000000, -1.000000000000000000 ) ) ;
#28034 = CARTESIAN_POINT ( 'NONE',  ( 157.4999999999998579, 181.1279373836408411, -45.00000000000000000 ) ) ;
#28035 = VERTEX_POINT ( 'NONE', #4238 ) ;
#28036 = FACE_OUTER_BOUND ( 'NONE', #7054, .T. ) ;
#28037 = ORIENTED_EDGE ( 'NONE', *, *, #13599, .F. ) ;
#28038 = AXIS2_PLACEMENT_3D ( 'NONE', #9077, #19991, #323 ) ;
#28039 = CARTESIAN_POINT ( 'NONE',  ( 65.00000000000000000, -120.0000000000000995, -69.99999999999998579 ) ) ;
#28040 = CARTESIAN_POINT ( 'NONE',  ( -174.7479038800345563, 112.7071446407698403, -28.86810097183760959 ) ) ;
#28041 = ORIENTED_EDGE ( 'NONE', *, *, #17709, .T. ) ;
#28042 = EDGE_CURVE ( 'NONE', #7826, #1981, #12740, .T. ) ;
#28043 = CIRCLE ( 'NONE', #27156, 6.204828372381208546 ) ;
#28044 = VECTOR ( 'NONE', #16862, 1000.000000000000000 ) ;
#28045 = EDGE_LOOP ( 'NONE', ( #1634, #5222, #26972, #19194 ) ) ;
#28046 = EDGE_CURVE ( 'NONE', #5196, #4740, #10999, .T. ) ;
#28047 = DIRECTION ( 'NONE',  ( 0.5804519453834686704, -0.8142945039115434547, 0.000000000000000000 ) ) ;
#28048 = VERTEX_POINT ( 'NONE', #21772 ) ;
#28049 = CIRCLE ( 'NONE', #16148, 17.93072811908088937 ) ;
#28050 = EDGE_CURVE ( 'NONE', #6070, #13530, #4658, .T. ) ;
#28051 = ORIENTED_EDGE ( 'NONE', *, *, #24162, .T. ) ;
#28052 = EDGE_LOOP ( 'NONE', ( #14228, #27139, #26609, #19084 ) ) ;
#28053 = LINE ( 'NONE', #25495, #20331 ) ;
#28054 = FACE_OUTER_BOUND ( 'NONE', #7582, .T. ) ;
#28055 = FACE_OUTER_BOUND ( 'NONE', #6090, .T. ) ;
#28056 = CARTESIAN_POINT ( 'NONE',  ( -207.5044420441007560, 75.59897387903042443, 45.00000000000000000 ) ) ;
#28057 = CARTESIAN_POINT ( 'NONE',  ( 119.1248245724174524, 204.0122708680763424, -100.0000000000000000 ) ) ;
#28058 = CYLINDRICAL_SURFACE ( 'NONE', #3456, 10.00000000000000888 ) ;
#28059 = CARTESIAN_POINT ( 'NONE',  ( -235.5446291276663828, 67.70753763449675944, -5.872244511705135395 ) ) ;
#28060 = EDGE_LOOP ( 'NONE', ( #20110, #25122, #19607, #756 ) ) ;
#28061 = AXIS2_PLACEMENT_3D ( 'NONE', #6769, #22002, #8936 ) ;
#28062 = FACE_OUTER_BOUND ( 'NONE', #3315, .T. ) ;
#28063 = PLANE ( 'NONE',  #12921 ) ;
#28065 = DIRECTION ( 'NONE',  ( 0.000000000000000000, 0.000000000000000000, 1.000000000000000000 ) ) ;
#28064 = AXIS2_PLACEMENT_3D ( 'NONE', #18202, #26655, #17619 ) ;
#28066 = CARTESIAN_POINT ( 'NONE',  ( 113.1867617905510173, 225.5391268416508694, -97.32202223992345580 ) ) ;
#28067 = AXIS2_PLACEMENT_3D ( 'NONE', #22867, #7645, #20705 ) ;
#28068 = ORIENTED_EDGE ( 'NONE', *, *, #4272, .T. ) ;
#28069 = CARTESIAN_POINT ( 'NONE',  ( 157.9999999999998010, 236.5551250525490161, 45.00000000000000000 ) ) ;
#28070 = VECTOR ( 'NONE', #17311, 1000.000000000000000 ) ;
#28071 = DIRECTION ( 'NONE',  ( 0.8660254037844394848, 0.4999999999999985012, 0.000000000000000000 ) ) ;
#28072 = DIRECTION ( 'NONE',  ( 1.000000000000000000, -0.000000000000000000, -0.000000000000000000 ) ) ;
#28073 = DIRECTION ( 'NONE',  ( 0.000000000000000000, 0.000000000000000000, -1.000000000000000000 ) ) ;
#28074 = CARTESIAN_POINT ( 'NONE',  ( 158.0000000000000284, 205.9527499549551806, -45.00000000000000000 ) ) ;
#28075 = FACE_OUTER_BOUND ( 'NONE', #15364, .T. ) ;
#28076 = VERTEX_POINT ( 'NONE', #21623 ) ;
#28077 = EDGE_CURVE ( 'NONE', #5655, #477, #6253, .T. ) ;
#28078 = DIRECTION ( 'NONE',  ( -0.000000000000000000, -0.000000000000000000, -1.000000000000000000 ) ) ;
#28079 = EDGE_LOOP ( 'NONE', ( #18987, #2152, #23685, #27690 ) ) ;
#28080 = CARTESIAN_POINT ( 'NONE',  ( -49.97791255360778706, 113.2029523930418975, -145.0000000000000000 ) ) ;
#28081 = ORIENTED_EDGE ( 'NONE', *, *, #4959, .T. ) ;
#28082 = AXIS2_PLACEMENT_3D ( 'NONE', #5286, #14068, #20654 ) ;
#28083 = EDGE_LOOP ( 'NONE', ( #21708, #3347, #11534, #25477 ) ) ;
#28084 = CARTESIAN_POINT ( 'NONE',  ( -77.63961834651543370, 136.2561492527889015, 15.18776799126392163 ) ) ;
#28085 = CIRCLE ( 'NONE', #26724, 6.025000000000002132 ) ;
#28086 = EDGE_CURVE ( 'NONE', #26198, #9545, #1936, .T. ) ;
#28087 = ORIENTED_EDGE ( 'NONE', *, *, #109, .T. ) ;
#28088 = VERTEX_POINT ( 'NONE', #28074 ) ;
#28089 = AXIS2_PLACEMENT_3D ( 'NONE', #21833, #10915, #5607 ) ;
#28090 = CARTESIAN_POINT ( 'NONE',  ( -219.9082363642798441, 137.1815813412079308, 12.98324324887168402 ) ) ;
#28091 = CARTESIAN_POINT ( 'NONE',  ( -155.5576584249185146, 121.6218958557625740, -21.26367854068186958 ) ) ;
#28092 = DIRECTION ( 'NONE',  ( 0.000000000000000000, 0.000000000000000000, -1.000000000000000000 ) ) ;
#28093 = VECTOR ( 'NONE', #14711, 1000.000000000000000 ) ;
#28094 = EDGE_CURVE ( 'NONE', #1213, #8138, #4513, .T. ) ;
#28095 = CARTESIAN_POINT ( 'NONE',  ( -142.3432792462832310, 127.5062405277896147, -16.40804776362093875 ) ) ;
#28096 = CARTESIAN_POINT ( 'NONE',  ( -263.5400929610141247, -171.3942524661753453, -89.83009453516376652 ) ) ;
#28097 = CARTESIAN_POINT ( 'NONE',  ( -260.0000000000001137, -167.0819201924624906, 90.00000000000001421 ) ) ;
#28098 = CARTESIAN_POINT ( 'NONE',  ( -212.5557490532361840, 88.28325300605492032, -22.89340189428408578 ) ) ;
#28099 = CARTESIAN_POINT ( 'NONE',  ( 133.6295840780252036, 249.9693091936576081, -150.8447356795924179 ) ) ;
#28100 = CARTESIAN_POINT ( 'NONE',  ( -268.1197270641252430, -170.6145491720722589, -94.20778360409461527 ) ) ;
#28101 = DIRECTION ( 'NONE',  ( 0.000000000000000000, -1.000000000000000000, 0.000000000000000000 ) ) ;
#28102 = LINE ( 'NONE', #26241, #14621 ) ;
#28103 = DIRECTION ( 'NONE',  ( 0.8916010070295715684, -0.4528218681378516353, 0.000000000000000000 ) ) ;
#28104 = ORIENTED_EDGE ( 'NONE', *, *, #8999, .T. ) ;
#28105 = EDGE_CURVE ( 'NONE', #8173, #23544, #26211, .T. ) ;
#28106 = VECTOR ( 'NONE', #2059, 1000.000000000000000 ) ;
#28107 = AXIS2_PLACEMENT_3D ( 'NONE', #16238, #5303, #14084 ) ;
#28108 = CARTESIAN_POINT ( 'NONE',  ( 114.9638101962909360, 140.0000000000000000, 98.73786388354261589 ) ) ;
#28109 = LINE ( 'NONE', #24240, #3876 ) ;
#28110 = DIRECTION ( 'NONE',  ( -0.000000000000000000, 1.000000000000000000, -1.387778780781445429E-16 ) ) ;
#28111 = AXIS2_PLACEMENT_3D ( 'NONE', #18062, #9009, #16058 ) ;
#28113 = ORIENTED_EDGE ( 'NONE', *, *, #11888, .F. ) ;
#28112 = EDGE_LOOP ( 'NONE', ( #5491, #11631 ) ) ;
#28114 = AXIS2_PLACEMENT_3D ( 'NONE', #6121, #13030, #12462 ) ;
#28115 = EDGE_CURVE ( 'NONE', #3252, #2009, #8698, .T. ) ;
#28116 = CARTESIAN_POINT ( 'NONE',  ( 105.5907556405606158, 242.1385898947462465, -29.32397797500748737 ) ) ;
#28117 = VERTEX_POINT ( 'NONE', #15319 ) ;
#28118 = ORIENTED_EDGE ( 'NONE', *, *, #2589, .T. ) ;
#28119 = VERTEX_POINT ( 'NONE', #6815 ) ;
#28120 = ORIENTED_EDGE ( 'NONE', *, *, #23521, .T. ) ;
#28121 = ORIENTED_EDGE ( 'NONE', *, *, #4531, .T. ) ;
#28122 = VERTEX_POINT ( 'NONE', #24072 ) ;
#28123 = VECTOR ( 'NONE', #5739, 1000.000000000000000 ) ;
#28124 = CARTESIAN_POINT ( 'NONE',  ( 0.000000000000000000, 0.000000000000000000, 25.00000000000000000 ) ) ;
#28125 = EDGE_CURVE ( 'NONE', #4623, #22496, #4375, .T. ) ;
#28126 = VECTOR ( 'NONE', #23460, 1000.000000000000000 ) ;
#28127 = EDGE_CURVE ( 'NONE', #6015, #10156, #17176, .T. ) ;
#28128 = CARTESIAN_POINT ( 'NONE',  ( 158.0000000000002842, 180.8739998798873501, 45.00000000000000000 ) ) ;
#28129 = AXIS2_PLACEMENT_3D ( 'NONE', #14318, #16473, #5688 ) ;
#28130 = DIRECTION ( 'NONE',  ( 0.000000000000000000, 0.000000000000000000, -1.000000000000000000 ) ) ;
#28131 = CARTESIAN_POINT ( 'NONE',  ( 158.0000000000000568, 201.4448749474510407, 45.00000000000000000 ) ) ;
#28132 = LINE ( 'NONE', #16949, #6646 ) ;
#28133 = FACE_OUTER_BOUND ( 'NONE', #17118, .T. ) ;
#28134 = CARTESIAN_POINT ( 'NONE',  ( 109.9999999999999005, 240.0000000000000284, -5.000000000000004441 ) ) ;
#28135 = EDGE_CURVE ( 'NONE', #23612, #23548, #19748, .T. ) ;
#28136 = EDGE_CURVE ( 'NONE', #26013, #12924, #17593, .T. ) ;
#28137 = DIRECTION ( 'NONE',  ( 0.000000000000000000, 0.000000000000000000, -1.000000000000000000 ) ) ;
#28138 = CARTESIAN_POINT ( 'NONE',  ( -207.7351949253619239, 74.89624901011349323, 43.85536788017862619 ) ) ;
#28139 = CARTESIAN_POINT ( 'NONE',  ( 158.0000000000005684, 151.2873747973098659, -45.00000000000000000 ) ) ;
#28140 = CARTESIAN_POINT ( 'NONE',  ( 157.4999999999996589, 281.4429376839215138, 45.00000000000000000 ) ) ;
#28141 = ORIENTED_EDGE ( 'NONE', *, *, #1540, .F. ) ;
#28142 = VECTOR ( 'NONE', #4996, 1000.000000000000000 ) ;
#28143 = CARTESIAN_POINT ( 'NONE',  ( -188.7947732573136648, 104.2412161718895476, 31.96204269770191431 ) ) ;
#28144 = PRODUCT ( 'Sliding Carriage', 'Sliding Carriage', '', ( #17383 ) ) ;
#28145 = CARTESIAN_POINT ( 'NONE',  ( -266.5933816631180662, -170.7896271858165278, -104.7207418755312744 ) ) ;
#28146 = ORIENTED_EDGE ( 'NONE', *, *, #9816, .F. ) ;
#28147 = EDGE_CURVE ( 'NONE', #23933, #9172, #17310, .T. ) ;
#28148 = AXIS2_PLACEMENT_3D ( 'NONE', #22584, #11818, #20557 ) ;
#28149 = EDGE_LOOP ( 'NONE', ( #12428, #15608, #19338, #5732 ) ) ;
#28150 = VERTEX_POINT ( 'NONE', #15459 ) ;
#28151 = DIRECTION ( 'NONE',  ( -1.000000000000000000, 0.000000000000000000, -0.000000000000000000 ) ) ;
#28152 = DIRECTION ( 'NONE',  ( -0.000000000000000000, 0.000000000000000000, -1.000000000000000000 ) ) ;
#28153 = ORIENTED_EDGE ( 'NONE', *, *, #9786, .T. ) ;
#28154 = EDGE_LOOP ( 'NONE', ( #20894, #18222, #1631, #612 ) ) ;
#28155 = CARTESIAN_POINT ( 'NONE',  ( 106.3487426207649236, 91.82653269718771583, -100.0000000000000142 ) ) ;
#28156 = MANIFOLD_SOLID_BREP ( 'Cut-Extrude13', #9978 ) ;
#28158 = CARTESIAN_POINT ( 'NONE',  ( 158.0000000000012790, 83.57474959461971764, -45.00000000000000000 ) ) ;
#28157 =( REPRESENTATION_RELATIONSHIP ('NONE','NONE', #11963, #18912 ) REPRESENTATION_RELATIONSHIP_WITH_TRANSFORMATION ( #13097 )SHAPE_REPRESENTATION_RELATIONSHIP( ) );
#28159 = CARTESIAN_POINT ( 'NONE',  ( 158.0000000000005400, 156.3031248123239436, 45.00000000000000000 ) ) ;
#28160 = ORIENTED_EDGE ( 'NONE', *, *, #10483, .T. ) ;
#28161 = CARTESIAN_POINT ( 'NONE',  ( -216.9923549404892071, 86.31376438289755981, 20.42942837940906742 ) ) ;
#28162 = ORIENTED_EDGE ( 'NONE', *, *, #28046, .T. ) ;
#28163 = VECTOR ( 'NONE', #11085, 1000.000000000000000 ) ;
#28164 = CARTESIAN_POINT ( 'NONE',  ( 232.4999999999996305, 133.0668745871126930, 30.86484227207697018 ) ) ;
#28165 = DIRECTION ( 'NONE',  ( -0.000000000000000000, 0.000000000000000000, -1.000000000000000000 ) ) ;
#28166 = VECTOR ( 'NONE', #13769, 999.9999999999998863 ) ;
#28167 = CARTESIAN_POINT ( 'NONE',  ( 160.1668614390261496, 203.6666592782660246, -139.1934629298939683 ) ) ;
#28168 = LINE ( 'NONE', #20094, #19771 ) ;
#28169 = ORIENTED_EDGE ( 'NONE', *, *, #9262, .F. ) ;
#28170 = LINE ( 'NONE', #24027, #10933 ) ;
#28171 = DIRECTION ( 'NONE',  ( 1.000000000000000000, 0.000000000000000000, -0.000000000000000000 ) ) ;
#28172 = DIRECTION ( 'NONE',  ( 0.8916010070300181001, -0.4528218681369723941, 0.000000000000000000 ) ) ;
#28173 = DIRECTION ( 'NONE',  ( -0.000000000000000000, -0.000000000000000000, -1.000000000000000000 ) ) ;
#28174 = ORIENTED_EDGE ( 'NONE', *, *, #22027, .T. ) ;
#28175 = CARTESIAN_POINT ( 'NONE',  ( -40.40953891503691153, 0.000000000000000000, 99.00000000000000000 ) ) ;
#28176 = EDGE_CURVE ( 'NONE', #2326, #9517, #24208, .T. ) ;
#28177 = CARTESIAN_POINT ( 'NONE',  ( -180.7604701752530332, 109.5394202030439317, 30.00180410819614352 ) ) ;
#28178 = CARTESIAN_POINT ( 'NONE',  ( -43.02437977270766822, 129.7200458115293031, -16.81627168235288394 ) ) ;
#28179 = CARTESIAN_POINT ( 'NONE',  ( 157.9999999999998010, 233.5393750375350237, 45.00000000000000000 ) ) ;
#28180 = ORIENTED_EDGE ( 'NONE', *, *, #27399, .F. ) ;
#28181 = CARTESIAN_POINT ( 'NONE',  ( 158.0000000000002842, 178.8739998798873216, 45.00000000000000000 ) ) ;
#28182 = ORIENTED_EDGE ( 'NONE', *, *, #17846, .T. ) ;
#28183 = VECTOR ( 'NONE', #18402, 1000.000000000000000 ) ;
#28184 = CARTESIAN_POINT ( 'NONE',  ( -155.5799833640026577, 121.6126019772860474, 21.27136890865478946 ) ) ;
#28185 = CARTESIAN_POINT ( 'NONE',  ( -172.9314056506308361, 113.6797141081297298, -28.12266984373487588 ) ) ;
#28186 = VERTEX_POINT ( 'NONE', #5090 ) ;
#28187 = VECTOR ( 'NONE', #1829, 1000.000000000000227 ) ;
#28188 = ORIENTED_EDGE ( 'NONE', *, *, #3209, .F. ) ;
#28189 = DIRECTION ( 'NONE',  ( -0.000000000000000000, -0.000000000000000000, -1.000000000000000000 ) ) ;
#28190 = ORIENTED_EDGE ( 'NONE', *, *, #8328, .T. ) ;
#28191 = ORIENTED_EDGE ( 'NONE', *, *, #21511, .T. ) ;
#28192 = ORIENTED_EDGE ( 'NONE', *, *, #14537, .F. ) ;
#28193 = DIRECTION ( 'NONE',  ( 0.000000000000000000, 0.000000000000000000, -1.000000000000000000 ) ) ;
#28194 = ADVANCED_FACE ( 'NONE', ( #24343 ), #27069, .F. ) ;
#28195 = CARTESIAN_POINT ( 'NONE',  ( 157.9999999999999147, 215.9842499849850697, -45.00000000000000000 ) ) ;
#28196 = LINE ( 'NONE', #8542, #7060 ) ;
#28197 = DIRECTION ( 'NONE',  ( 0.2499999999999988898, 0.000000000000000000, -0.9682458365518545884 ) ) ;
#28198 = VECTOR ( 'NONE', #19769, 1000.000000000000000 ) ;
#28199 = AXIS2_PLACEMENT_3D ( 'NONE', #8302, #5575, #14491 ) ;
#28200 = CARTESIAN_POINT ( 'NONE',  ( -277.2150368962633706, -170.0000000000001137, 101.5769467933889558 ) ) ;
#28201 = DIRECTION ( 'NONE',  ( -1.000000000000000000, 0.000000000000000000, 0.000000000000000000 ) ) ;
#28202 = CARTESIAN_POINT ( 'NONE',  ( -222.1142713348111783, 61.47487629661259945, -10.02481564198514619 ) ) ;
#28203 = ORIENTED_EDGE ( 'NONE', *, *, #7062, .T. ) ;
#28204 = CARTESIAN_POINT ( 'NONE',  ( 112.4999999999998863, 220.0000000000000284, -99.00000000000001421 ) ) ;
#28205 = EDGE_CURVE ( 'NONE', #23090, #8779, #23471, .T. ) ;
#28206 = VECTOR ( 'NONE', #9381, 1000.000000000000000 ) ;
#28207 = FACE_OUTER_BOUND ( 'NONE', #23424, .T. ) ;
#28208 = DIRECTION ( 'NONE',  ( 0.4528218681380914989, 0.8916010070294497769, -0.000000000000000000 ) ) ;
#28209 = CARTESIAN_POINT ( 'NONE',  ( 157.9999999999998295, 229.0315000300280417, -45.00000000000000000 ) ) ;
#28210 = EDGE_LOOP ( 'NONE', ( #21097, #10782, #19376, #1596 ) ) ;
#28211 = EDGE_CURVE ( 'NONE', #19047, #24186, #9695, .T. ) ;
#28212 = CARTESIAN_POINT ( 'NONE',  ( 89.99999999999994316, -40.00000000000002132, -70.00000000000001421 ) ) ;
#28213 = ADVANCED_FACE ( 'NONE', ( #9122 ), #17883, .F. ) ;
#28214 = EDGE_CURVE ( 'NONE', #17712, #5857, #5235, .T. ) ;
#28215 = DIRECTION ( 'NONE',  ( -0.000000000000000000, -0.000000000000000000, -1.000000000000000000 ) ) ;
#28216 = FACE_OUTER_BOUND ( 'NONE', #4000, .T. ) ;
#28217 = CARTESIAN_POINT ( 'NONE',  ( 158.0000000000007674, 131.2243747372535267, -45.00000000000000000 ) ) ;
#28218 = DIRECTION ( 'NONE',  ( 0.000000000000000000, -1.000000000000000000, 0.000000000000000000 ) ) ;
#28219 = LINE ( 'NONE', #4096, #12499 ) ;
#28220 = VERTEX_POINT ( 'NONE', #14024 ) ;
#28221 = DIRECTION ( 'NONE',  ( 1.000000000000000000, 1.321694076934710155E-16, -0.000000000000000000 ) ) ;
#28222 = ORIENTED_EDGE ( 'NONE', *, *, #9327, .T. ) ;
#28223 = CARTESIAN_POINT ( 'NONE',  ( -279.1278187736259611, -165.0000000000001421, 106.1966075482099399 ) ) ;
#28224 = EDGE_LOOP ( 'NONE', ( #26963, #14504, #21852, #21125 ) ) ;
#28225 = CIRCLE ( 'NONE', #15875, 58.90601976618767566 ) ;
#28226 = EDGE_LOOP ( 'NONE', ( #25269, #17803, #16077, #7915 ) ) ;
#28227 = DIRECTION ( 'NONE',  ( -0.000000000000000000, -0.000000000000000000, -1.000000000000000000 ) ) ;
#28228 = ORIENTED_EDGE ( 'NONE', *, *, #5449, .T. ) ;
#28229 = AXIS2_PLACEMENT_3D ( 'NONE', #17720, #2196, #26335 ) ;
#28230 = EDGE_LOOP ( 'NONE', ( #24877, #10762, #15759, #22088 ) ) ;
#28231 = DIRECTION ( 'NONE',  ( 1.000000000000000000, 0.000000000000000000, 0.000000000000000000 ) ) ;
#28232 = CARTESIAN_POINT ( 'NONE',  ( 158.0000000000012790, 83.57474959461971764, 45.00000000000000000 ) ) ;
#28233 = FACE_OUTER_BOUND ( 'NONE', #4284, .T. ) ;
#28234 = CARTESIAN_POINT ( 'NONE',  ( 158.0000000000017337, 40.94087446699997912, -45.00000000000000000 ) ) ;
#28235 = CARTESIAN_POINT ( 'NONE',  ( -160.0000000000000568, 90.00000000000001421, 110.0000000000000284 ) ) ;
#28236 = EDGE_CURVE ( 'NONE', #12526, #24450, #13589, .T. ) ;
#28237 = CARTESIAN_POINT ( 'NONE',  ( -261.2693309676747617, -166.7184184611137709, -89.99999999999987210 ) ) ;
#28238 = ADVANCED_FACE ( 'NONE', ( #15893 ), #24493, .F. ) ;
#28239 = CARTESIAN_POINT ( 'NONE',  ( -268.1741054074460635, -165.4056554755341892, 88.87211405343852277 ) ) ;
#28240 = CARTESIAN_POINT ( 'NONE',  ( -224.4622899665858711, 89.01046014348733593, -16.48139453409665833 ) ) ;
#28241 = CARTESIAN_POINT ( 'NONE',  ( 217.4999999999996305, 258.6181251126050711, -5.999999999999991118 ) ) ;
#28242 = CIRCLE ( 'NONE', #3011, 5.000000000000000888 ) ;
#28243 = LINE ( 'NONE', #11314, #11739 ) ;
#28244 = CARTESIAN_POINT ( 'NONE',  ( 89.99999999999994316, -90.00000000000001421, -70.00000000000001421 ) ) ;
#28245 = DIRECTION ( 'NONE',  ( -1.000000000000000000, 0.000000000000000000, -9.251858538542972814E-17 ) ) ;
#28246 = FACE_OUTER_BOUND ( 'NONE', #16937, .T. ) ;
#28247 = VECTOR ( 'NONE', #11149, 1000.000000000000000 ) ;
#28248 = ORIENTED_EDGE ( 'NONE', *, *, #1563, .T. ) ;
#28249 = CARTESIAN_POINT ( 'NONE',  ( 79.99999999999992895, 110.0000000000000000, 45.00000000000000000 ) ) ;
#28250 = EDGE_CURVE ( 'NONE', #15878, #3625, #22772, .T. ) ;
#28251 = DIRECTION ( 'NONE',  ( -1.000000000000000000, 0.000000000000000000, 0.000000000000000000 ) ) ;
#28252 = DIRECTION ( 'NONE',  ( 1.000000000000000000, -0.000000000000000000, -0.000000000000000000 ) ) ;
#28253 = CARTESIAN_POINT ( 'NONE',  ( 106.6102839382104719, 210.3032261119582813, -146.5591841905930721 ) ) ;
#28254 = VECTOR ( 'NONE', #22963, 1000.000000000000000 ) ;
#28255 = ORIENTED_EDGE ( 'NONE', *, *, #25375, .F. ) ;
#28256 = ADVANCED_FACE ( 'NONE', ( #26933 ), #11434, .F. ) ;
#28257 = CARTESIAN_POINT ( 'NONE',  ( 89.37316688736883918, 230.0797033051251788, -16.48577246127781493 ) ) ;
#28258 = EDGE_LOOP ( 'NONE', ( #14398, #20352, #26262, #20579 ) ) ;
#28259 = CARTESIAN_POINT ( 'NONE',  ( -38.16446318061785092, 129.9977304598137948, -15.32283089668279530 ) ) ;
#28260 = ORIENTED_EDGE ( 'NONE', *, *, #15595, .F. ) ;
#28261 = EDGE_LOOP ( 'NONE', ( #4313, #15502, #9668, #15818 ) ) ;
#28262 = ORIENTED_EDGE ( 'NONE', *, *, #52, .F. ) ;
#28263 = EDGE_LOOP ( 'NONE', ( #17641, #25183, #21952, #2547 ) ) ;
#28264 = ORIENTED_EDGE ( 'NONE', *, *, #16537, .T. ) ;
#28265 = AXIS2_PLACEMENT_3D ( 'NONE', #24008, #6046, #23864 ) ;
#28266 = DIRECTION ( 'NONE',  ( 0.000000000000000000, 0.000000000000000000, 1.000000000000000000 ) ) ;
#28267 = PLANE ( 'NONE',  #21078 ) ;
#28268 = VECTOR ( 'NONE', #4263, 1000.000000000000000 ) ;
#28269 = CARTESIAN_POINT ( 'NONE',  ( 157.9999999999997158, 258.6181251126050711, 45.00000000000000000 ) ) ;
#28270 = DIRECTION ( 'NONE',  ( 0.7071067811865514585, -0.000000000000000000, 0.7071067811865435759 ) ) ;
#28271 = EDGE_CURVE ( 'NONE', #4562, #14563, #9418, .T. ) ;
#28272 = FACE_OUTER_BOUND ( 'NONE', #21103, .T. ) ;
#28273 = CARTESIAN_POINT ( 'NONE',  ( 124.9999999999998579, 220.0000000000000284, 45.00000000000000000 ) ) ;
#28274 = CARTESIAN_POINT ( 'NONE',  ( -277.2150368962633706, -237.2150368962634559, -110.0000000000000284 ) ) ;
#28275 = CARTESIAN_POINT ( 'NONE',  ( 89.99999999999988631, 260.0000000000000000, 15.00000000000000000 ) ) ;
#28276 = DIRECTION ( 'NONE',  ( 0.000000000000000000, -0.000000000000000000, 1.000000000000000000 ) ) ;
#28277 = DIRECTION ( 'NONE',  ( 0.000000000000000000, 0.000000000000000000, -1.000000000000000000 ) ) ;
#28278 = LINE ( 'NONE', #6176, #27556 ) ;
#28279 = DIRECTION ( 'NONE',  ( -1.000000000000000000, 6.167905692361982533E-16, 1.850371707708594760E-15 ) ) ;
#28281 = EDGE_LOOP ( 'NONE', ( #18075, #26000, #7041, #16243 ) ) ;
#28280 = VERTEX_POINT ( 'NONE', #22632 ) ;
#28282 = AXIS2_PLACEMENT_3D ( 'NONE', #27902, #9985, #1767 ) ;
#28283 = DIRECTION ( 'NONE',  ( -0.000000000000000000, 1.000000000000000000, -0.000000000000000000 ) ) ;
#28284 = EDGE_CURVE ( 'NONE', #15009, #4982, #7403, .T. ) ;
#28285 = EDGE_CURVE ( 'NONE', #25380, #1111, #11725, .T. ) ;
#28286 = CARTESIAN_POINT ( 'NONE',  ( -263.8977010603396138, -171.2736078107176638, -104.9999999999167812 ) ) ;
#28287 = ORIENTED_EDGE ( 'NONE', *, *, #21515, .T. ) ;
#28288 = APPLICATION_PROTOCOL_DEFINITION ( 'draft international standard', 'automotive_design', 1998, #15356 ) ;
#28289 = VERTEX_POINT ( 'NONE', #16169 ) ;
#28290 = ORIENTED_EDGE ( 'NONE', *, *, #15132, .T. ) ;
#28291 = LINE ( 'NONE', #11221, #13901 ) ;
#28292 = DIRECTION ( 'NONE',  ( -0.8916010070293383105, -0.4528218681383106015, 0.000000000000000000 ) ) ;
#28293 = ORIENTED_EDGE ( 'NONE', *, *, #26503, .T. ) ;
#28294 = EDGE_CURVE ( 'NONE', #15527, #18881, #14570, .T. ) ;
#28295 = CARTESIAN_POINT ( 'NONE',  ( 104.1118574116271418, 122.0584436054305684, -99.99999999997839950 ) ) ;
#28296 = EDGE_CURVE ( 'NONE', #8138, #8166, #16584, .T. ) ;
#28297 = DIRECTION ( 'NONE',  ( -0.8916010070297244461, -0.4528218681375507093, 0.000000000000000000 ) ) ;
#28298 = ORIENTED_EDGE ( 'NONE', *, *, #19, .T. ) ;
#28299 = CARTESIAN_POINT ( 'NONE',  ( -217.9474420836749289, 87.77798100153485450, 17.55735672534662228 ) ) ;
#28300 = ORIENTED_EDGE ( 'NONE', *, *, #27823, .T. ) ;
#28301 = CARTESIAN_POINT ( 'NONE',  ( -212.9132412317957233, -217.4562798785298128, 105.7556772048274922 ) ) ;
#28302 = DIRECTION ( 'NONE',  ( -0.000000000000000000, 0.000000000000000000, 1.000000000000000000 ) ) ;
#28303 = DIRECTION ( 'NONE',  ( 0.000000000000000000, 0.000000000000000000, -1.000000000000000000 ) ) ;
#28304 = CARTESIAN_POINT ( 'NONE',  ( 267.4999999999996021, 194.4107529906318064, 288.0938197134494203 ) ) ;
#28305 = ORIENTED_EDGE ( 'NONE', *, *, #25834, .T. ) ;
#28306 = CARTESIAN_POINT ( 'NONE',  ( 116.8936292565948776, 206.6308718070802684, 99.51164200157786865 ) ) ;
#28307 = CARTESIAN_POINT ( 'NONE',  ( 157.9999999999997442, 251.6023750975910218, -45.00000000000000000 ) ) ;
#28308 = CARTESIAN_POINT ( 'NONE',  ( 157.4999999999996589, 276.4271876689075498, 45.00000000000000000 ) ) ;
#28309 = CARTESIAN_POINT ( 'NONE',  ( 157.4999999999998579, 53.22631200078164682, -45.00000000000000000 ) ) ;
#28310 = ORIENTED_EDGE ( 'NONE', *, *, #17289, .F. ) ;
#28311 = CARTESIAN_POINT ( 'NONE',  ( -212.0383327733632370, -220.0000000000000284, -106.4038250379320516 ) ) ;
#28312 = EDGE_CURVE ( 'NONE', #8626, #5381, #25609, .T. ) ;
#28313 = AXIS2_PLACEMENT_3D ( 'NONE', #2168, #26163, #28303 ) ;
#28314 = EDGE_CURVE ( 'NONE', #2370, #14118, #14765, .T. ) ;
#28315 = CARTESIAN_POINT ( 'NONE',  ( -164.5581833258768825, 118.4903777742713658, 22.95450677488445024 ) ) ;
#28316 = CARTESIAN_POINT ( 'NONE',  ( -221.7385414042798573, 88.25646530137930768, 15.53772012378376566 ) ) ;
#28317 = ORIENTED_EDGE ( 'NONE', *, *, #20357, .F. ) ;
#28318 = ORIENTED_EDGE ( 'NONE', *, *, #23327, .F. ) ;
#28319 = VECTOR ( 'NONE', #25526, 1000.000000000000000 ) ;
#28320 = CARTESIAN_POINT ( 'NONE',  ( -190.0000000000000284, -40.00000000000004974, 110.0000000000000284 ) ) ;
#28321 = CARTESIAN_POINT ( 'NONE',  ( -186.6633805910676642, 105.4812463994875884, -32.52244268913835867 ) ) ;
#28322 = EDGE_LOOP ( 'NONE', ( #1898, #16183, #10349, #12714 ) ) ;
#28324 = VERTEX_POINT ( 'NONE', #5936 ) ;
#28323 = ADVANCED_FACE ( 'NONE', ( #25195 ), #12283, .F. ) ;
#28325 = CARTESIAN_POINT ( 'NONE',  ( 144.9999999999998863, 220.0000000000000284, -90.00000000000002842 ) ) ;
#28326 = CARTESIAN_POINT ( 'NONE',  ( 4.996003610813208850E-14, -120.0000000000001137, 25.00000000000000000 ) ) ;
#28327 = ORIENTED_EDGE ( 'NONE', *, *, #15350, .F. ) ;
#28328 = ORIENTED_EDGE ( 'NONE', *, *, #13321, .F. ) ;
#28329 = ADVANCED_FACE ( 'NONE', ( #14433 ), #23045, .F. ) ;
#28330 = LINE ( 'NONE', #197, #11637 ) ;
#28331 = EDGE_CURVE ( 'NONE', #3105, #18450, #14710, .T. ) ;
#28332 = CIRCLE ( 'NONE', #20545, 30.49120955644046660 ) ;
#28333 = TOROIDAL_SURFACE ( 'NONE', #17794, 14.95564396479129243, 3.532530335305412716 ) ;
#28334 = CARTESIAN_POINT ( 'NONE',  ( 134.9999999999998579, 220.0000000000000284, -90.00000000000002842 ) ) ;
#28335 = EDGE_CURVE ( 'NONE', #1943, #23236, #27478, .T. ) ;
#28336 = LINE ( 'NONE', #6517, #8439 ) ;
#28337 = CARTESIAN_POINT ( 'NONE',  ( 20.92655468430566756, 155.3461090732848220, -15.00000000000000000 ) ) ;
#28338 = CARTESIAN_POINT ( 'NONE',  ( 134.9999999999998579, 220.0000000000000284, 109.9999999999999858 ) ) ;
#28339 = DIRECTION ( 'NONE',  ( 0.4528218681383056610, -0.8916010070293409751, 0.000000000000000000 ) ) ;
#28340 = ORIENTED_EDGE ( 'NONE', *, *, #23253, .F. ) ;
#28341 = PLANE ( 'NONE',  #13628 ) ;
#28342 = CARTESIAN_POINT ( 'NONE',  ( 157.4999999999996589, 273.9193126614005678, -45.00000000000000000 ) ) ;
#28343 = CARTESIAN_POINT ( 'NONE',  ( 157.9999999999998010, 231.5393750375350237, 45.00000000000000000 ) ) ;
#28344 = CARTESIAN_POINT ( 'NONE',  ( 157.9999999999998295, 228.5236250225210313, -45.00000000000000000 ) ) ;
#28345 = ORIENTED_EDGE ( 'NONE', *, *, #22006, .F. ) ;
#28346 = LINE ( 'NONE', #6951, #20143 ) ;
#28347 = CARTESIAN_POINT ( 'NONE',  ( -28.05246235954390244, 188.0718642840173516, -15.00000000000000000 ) ) ;
#28348 = CARTESIAN_POINT ( 'NONE',  ( 367.4999999999996021, 44.41075299063186321, -100.0000000000000142 ) ) ;
#28349 = DIRECTION ( 'NONE',  ( 0.4528218681376312005, -0.8916010070296835899, 0.000000000000000000 ) ) ;
#28350 = DIRECTION ( 'NONE',  ( -0.8916010070299273949, -0.4528218681371510845, 0.000000000000000000 ) ) ;
#28351 = ORIENTED_EDGE ( 'NONE', *, *, #9592, .F. ) ;
#28352 = AXIS2_PLACEMENT_3D ( 'NONE', #1375, #12170, #16884 ) ;
#28353 = CARTESIAN_POINT ( 'NONE',  ( 157.9999999999997158, 261.1260001201120531, -45.00000000000000000 ) ) ;
#28354 = EDGE_LOOP ( 'NONE', ( #18312, #10900, #17875, #8455 ) ) ;
#28355 = DIRECTION ( 'NONE',  ( -1.000000000000000000, -0.000000000000000000, -0.000000000000000000 ) ) ;
#28356 = CIRCLE ( 'NONE', #7290, 75.00000000000002842 ) ;
#28357 = ORIENTED_EDGE ( 'NONE', *, *, #10649, .F. ) ;
#28358 = VERTEX_POINT ( 'NONE', #7958 ) ;
#28359 = DIRECTION ( 'NONE',  ( 0.8916010070295309342, -0.4528218681379315713, 0.000000000000000000 ) ) ;
#28360 = ORIENTED_EDGE ( 'NONE', *, *, #24154, .F. ) ;
#28361 = EDGE_CURVE ( 'NONE', #19423, #1670, #1069, .T. ) ;
#28362 = ORIENTED_EDGE ( 'NONE', *, *, #24762, .F. ) ;
#28363 = DIRECTION ( 'NONE',  ( 0.000000000000000000, 0.000000000000000000, 1.000000000000000000 ) ) ;
#28364 = CARTESIAN_POINT ( 'NONE',  ( -212.9132412317957233, -217.4562798785298128, 94.24432279517255040 ) ) ;
#28365 = EDGE_CURVE ( 'NONE', #27215, #17603, #11559, .T. ) ;
#28366 = AXIS2_PLACEMENT_3D ( 'NONE', #5328, #9371, #24588 ) ;
#28367 = ADVANCED_FACE ( 'NONE', ( #1486 ), #27340, .F. ) ;
#28368 = CARTESIAN_POINT ( 'NONE',  ( 47.90501010967909679, 226.8374036014029969, 45.00000000000000000 ) ) ;
#28369 = DIRECTION ( 'NONE',  ( 0.000000000000000000, 0.000000000000000000, 1.000000000000000000 ) ) ;
#28370 = DIRECTION ( 'NONE',  ( -0.6787614006938686995, -0.7343588774761953264, 0.000000000000000000 ) ) ;
#28371 = AXIS2_PLACEMENT_3D ( 'NONE', #14952, #1854, #24137 ) ;
#28372 = LINE ( 'NONE', #17618, #14473 ) ;
#28373 = CARTESIAN_POINT ( 'NONE',  ( -215.0361879928736073, 86.55905346095244113, -21.66337491047849895 ) ) ;
#28374 = CARTESIAN_POINT ( 'NONE',  ( 0.6601832576045314482, -1.249999999999998890, -7.428391153593958407 ) ) ;
#28375 = VECTOR ( 'NONE', #17088, 1000.000000000000000 ) ;
#28376 = DIRECTION ( 'NONE',  ( 0.000000000000000000, 1.000000000000000000, 0.000000000000000000 ) ) ;
#28377 = DIRECTION ( 'NONE',  ( 1.000000000000000000, 8.673617379884036705E-17, 0.000000000000000000 ) ) ;
#28378 = CARTESIAN_POINT ( 'NONE',  ( -189.8086322075389774, 92.49158130768422836, -13.00000000000000000 ) ) ;
#28379 = DIRECTION ( 'NONE',  ( 0.000000000000000000, -1.000000000000000000, 0.000000000000000000 ) ) ;
#28380 = ORIENTED_EDGE ( 'NONE', *, *, #21386, .F. ) ;
#28381 = CARTESIAN_POINT ( 'NONE',  ( 158.0000000000003695, 173.3503748573662051, 45.00000000000000000 ) ) ;
#28382 = DIRECTION ( 'NONE',  ( 0.000000000000000000, 0.000000000000000000, -1.000000000000000000 ) ) ;
#28383 = CARTESIAN_POINT ( 'NONE',  ( 158.0000000000009663, 111.1613746771971876, -45.00000000000000000 ) ) ;
#28384 = FACE_OUTER_BOUND ( 'NONE', #11999, .T. ) ;
#28385 = ORIENTED_EDGE ( 'NONE', *, *, #794, .F. ) ;
#28386 = VECTOR ( 'NONE', #13434, 1000.000000000000000 ) ;
#28387 = CARTESIAN_POINT ( 'NONE',  ( 88.44954299047357438, 230.0000000005625225, -16.19779584935188055 ) ) ;
#28388 = EDGE_LOOP ( 'NONE', ( #9959, #9024, #17149, #2942 ) ) ;
#28389 = CARTESIAN_POINT ( 'NONE',  ( -23.72680257353332678, 129.3221895177523777, -15.61617233342094302 ) ) ;
#28390 = ORIENTED_EDGE ( 'NONE', *, *, #27273, .T. ) ;
#28391 = AXIS2_PLACEMENT_3D ( 'NONE', #18152, #26906, #7658 ) ;
#28392 = ORIENTED_EDGE ( 'NONE', *, *, #3548, .F. ) ;
#28393 = AXIS2_PLACEMENT_3D ( 'NONE', #15491, #8730, #17206 ) ;
#28394 = EDGE_CURVE ( 'NONE', #20507, #6925, #2359, .T. ) ;
#28395 = EDGE_LOOP ( 'NONE', ( #12254, #27036, #14289, #2262, #10732, #25943, #12271, #6287, #12252, #9599, #2620, #16347, #9672, #20074, #4815 ) ) ;
#28396 = ORIENTED_EDGE ( 'NONE', *, *, #27074, .F. ) ;
#28397 = ORIENTED_EDGE ( 'NONE', *, *, #23602, .F. ) ;
#28398 = CARTESIAN_POINT ( 'NONE',  ( 89.99999999999994316, -40.00000000000002842, -100.0000000000000142 ) ) ;
#28399 = CARTESIAN_POINT ( 'NONE',  ( -40.48066117626728300, 130.4479960067108095, 16.52331096680928368 ) ) ;
#28400 = NEXT_ASSEMBLY_USAGE_OCCURRENCE ( 'NAUO1', ' ', ' ', #16857, #13176, $ ) ;
#28401 = NEXT_ASSEMBLY_USAGE_OCCURRENCE ( 'NAUO2', ' ', ' ', #16857, #1224, $ ) ;
#28402 = NEXT_ASSEMBLY_USAGE_OCCURRENCE ( 'NAUO3', ' ', ' ', #16857, #3316, $ ) ;
#28403 = NEXT_ASSEMBLY_USAGE_OCCURRENCE ( 'NAUO4', ' ', ' ', #16857, #20363, $ ) ;
#28404 = NEXT_ASSEMBLY_USAGE_OCCURRENCE ( 'NAUO5', ' ', ' ', #16857, #6305, $ ) ;
#28405 = NEXT_ASSEMBLY_USAGE_OCCURRENCE ( 'NAUO6', ' ', ' ', #16857, #8432, $ ) ;
#28406 = NEXT_ASSEMBLY_USAGE_OCCURRENCE ( 'NAUO7', ' ', ' ', #16857, #186, $ ) ;
#28407 = NEXT_ASSEMBLY_USAGE_OCCURRENCE ( 'NAUO8', ' ', ' ', #16857, #18451, $ ) ;
#28408 = NEXT_ASSEMBLY_USAGE_OCCURRENCE ( 'NAUO9', ' ', ' ', #16857, #25635, $ ) ;
#28409 = NEXT_ASSEMBLY_USAGE_OCCURRENCE ( 'NAUO10', ' ', ' ', #16857, #25635, $ ) ;
#28410 = NEXT_ASSEMBLY_USAGE_OCCURRENCE ( 'NAUO11', ' ', ' ', #16857, #25635, $ ) ;
#28411 = NEXT_ASSEMBLY_USAGE_OCCURRENCE ( 'NAUO12', ' ', ' ', #16857, #25635, $ ) ;
#28412 = NEXT_ASSEMBLY_USAGE_OCCURRENCE ( 'NAUO13', ' ', ' ', #16857, #25635, $ ) ;
#28413 = NEXT_ASSEMBLY_USAGE_OCCURRENCE ( 'NAUO14', ' ', ' ', #16857, #25635, $ ) ;
#28414=COLOUR_RGB('Dark Blue',0.08,0.2,0.34);
#28415=FILL_AREA_STYLE_COLOUR('',#28414);
#28416=FILL_AREA_STYLE('',(#28415));
#28417=SURFACE_STYLE_FILL_AREA(#28416);
#28418=SURFACE_SIDE_STYLE('',(#28417));
#28419=SURFACE_STYLE_USAGE(.BOTH.,#28418);
#28420=PRESENTATION_STYLE_ASSIGNMENT((#28419));
#28421=COLOUR_RGB('Light Blue',0.38,0.62,0.78);
#28422=FILL_AREA_STYLE_COLOUR('',#28421);
#28423=FILL_AREA_STYLE('',(#28422));
#28424=SURFACE_STYLE_FILL_AREA(#28423);
#28425=SURFACE_SIDE_STYLE('',(#28424));
#28426=SURFACE_STYLE_USAGE(.BOTH.,#28425);
#28427=PRESENTATION_STYLE_ASSIGNMENT((#28426));
#28428=COLOUR_RGB('Sky Blue',0.24,0.69,0.87);
#28429=FILL_AREA_STYLE_COLOUR('',#28428);
#28430=FILL_AREA_STYLE('',(#28429));
#28431=SURFACE_STYLE_FILL_AREA(#28430);
#28432=SURFACE_SIDE_STYLE('',(#28431));
#28433=SURFACE_STYLE_USAGE(.BOTH.,#28432);
#28434=PRESENTATION_STYLE_ASSIGNMENT((#28433));
#28435=COLOUR_RGB('Grey',0.48,0.52,0.57);
#28436=FILL_AREA_STYLE_COLOUR('',#28435);
#28437=FILL_AREA_STYLE('',(#28436));
#28438=SURFACE_STYLE_FILL_AREA(#28437);
#28439=SURFACE_SIDE_STYLE('',(#28438));
#28440=SURFACE_STYLE_USAGE(.BOTH.,#28439);
#28441=PRESENTATION_STYLE_ASSIGNMENT((#28440));
#28442=COLOUR_RGB('Black',0.12,0.14,0.17);
#28443=FILL_AREA_STYLE_COLOUR('',#28442);
#28444=FILL_AREA_STYLE('',(#28443));
#28445=SURFACE_STYLE_FILL_AREA(#28444);
#28446=SURFACE_SIDE_STYLE('',(#28445));
#28447=SURFACE_STYLE_USAGE(.BOTH.,#28446);
#28448=PRESENTATION_STYLE_ASSIGNMENT((#28447));
#28449=COLOUR_RGB('Off White',0.89,0.88,0.83);
#28450=FILL_AREA_STYLE_COLOUR('',#28449);
#28451=FILL_AREA_STYLE('',(#28450));
#28452=SURFACE_STYLE_FILL_AREA(#28451);
#28453=SURFACE_SIDE_STYLE('',(#28452));
#28454=SURFACE_STYLE_USAGE(.BOTH.,#28453);
#28455=PRESENTATION_STYLE_ASSIGNMENT((#28454));
ENDSEC;
END-ISO-10303-21;
